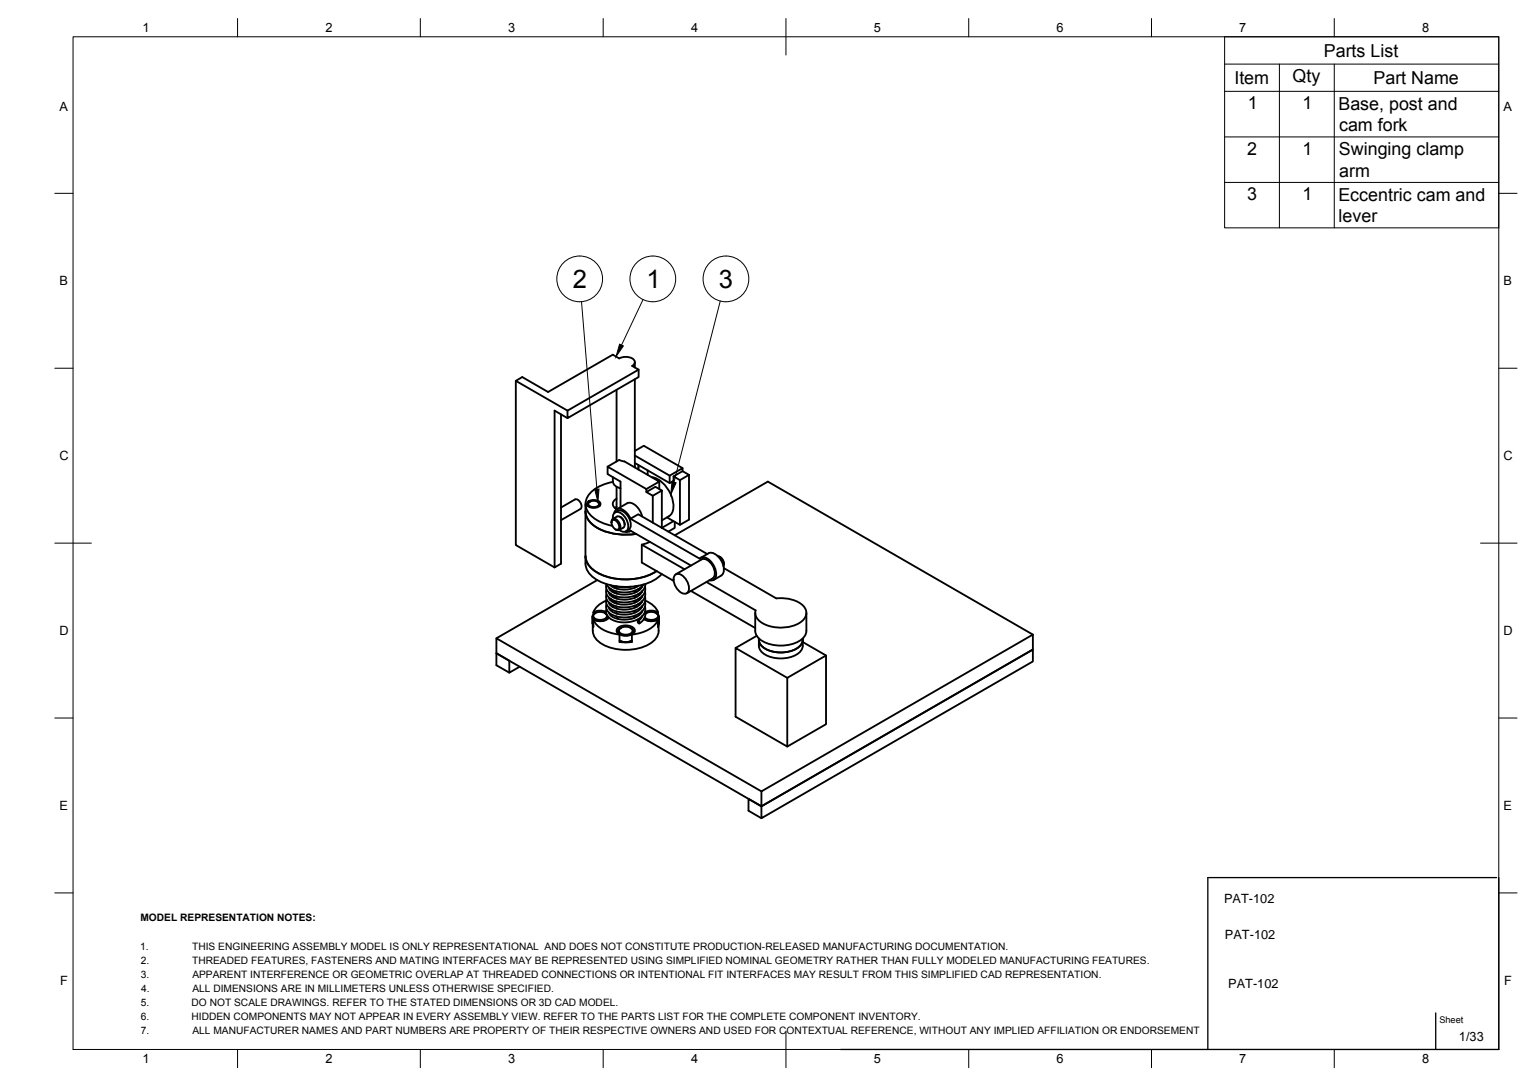
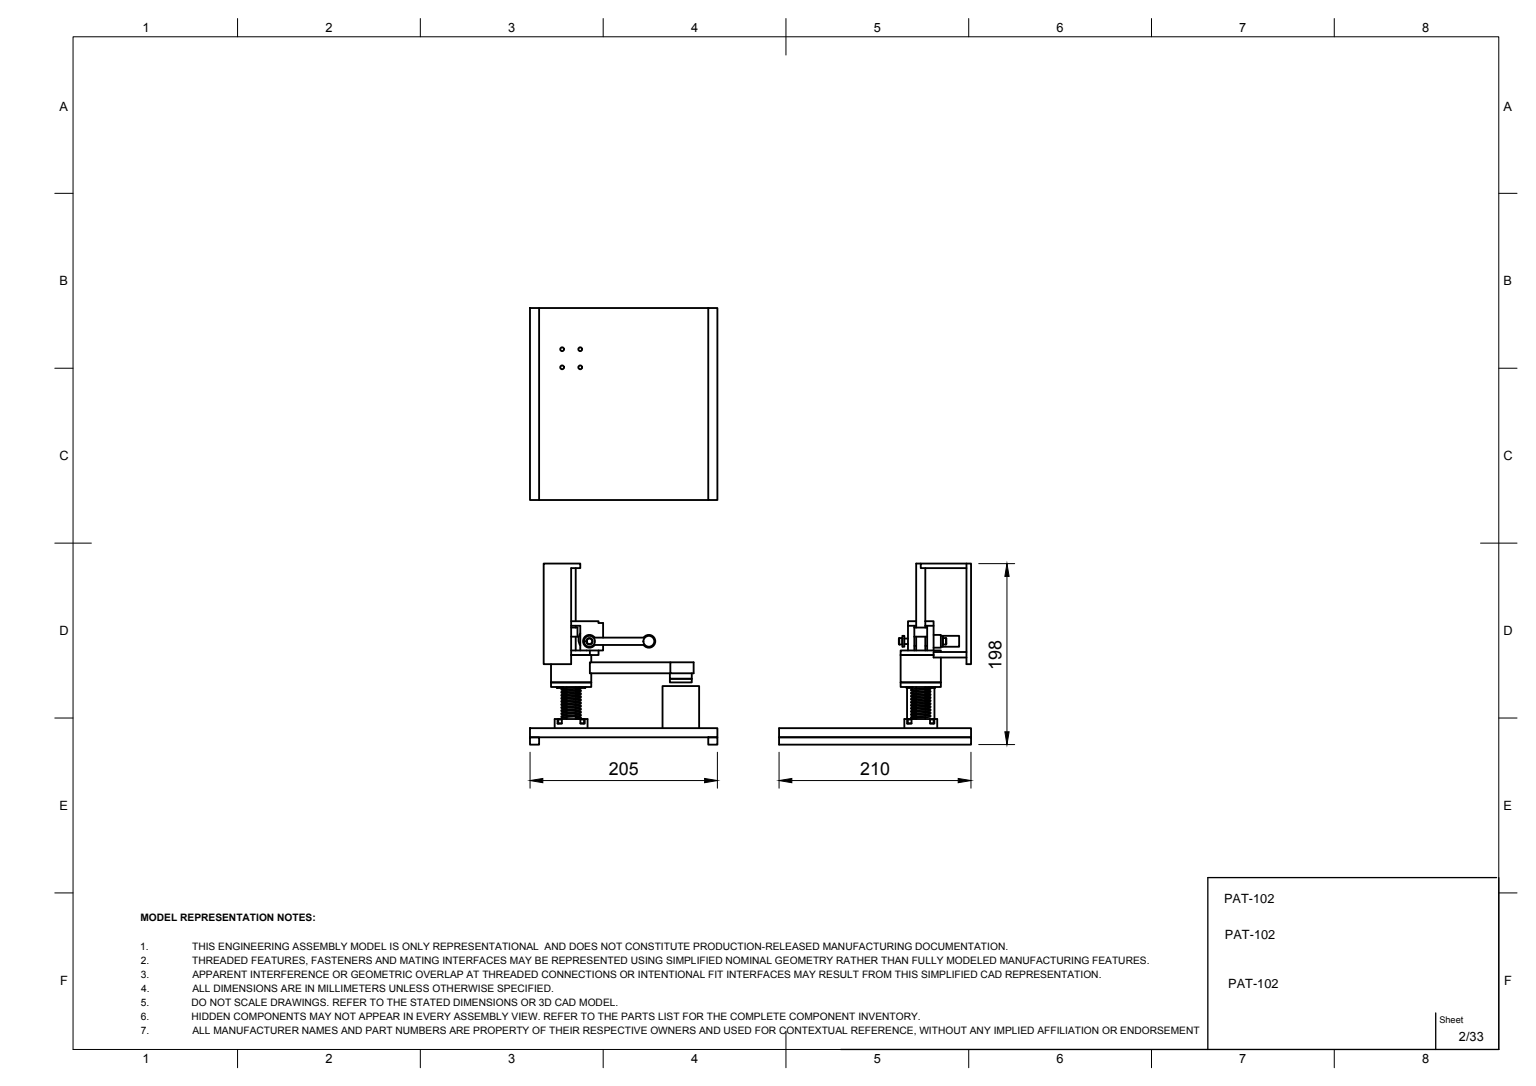
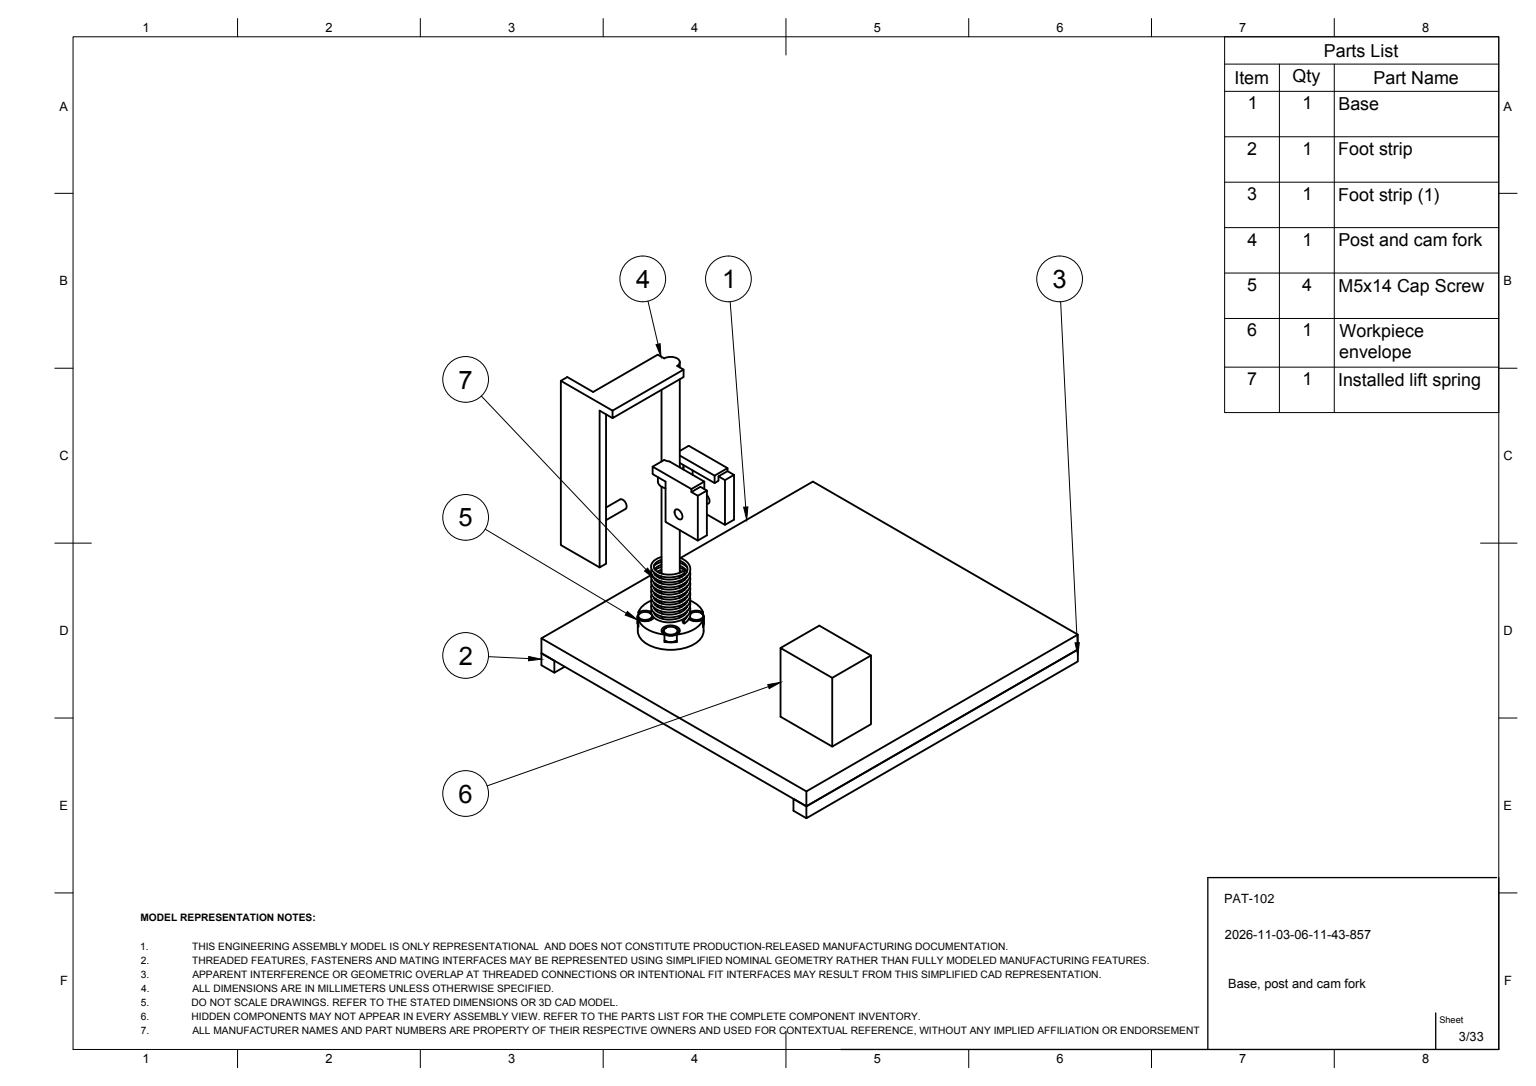
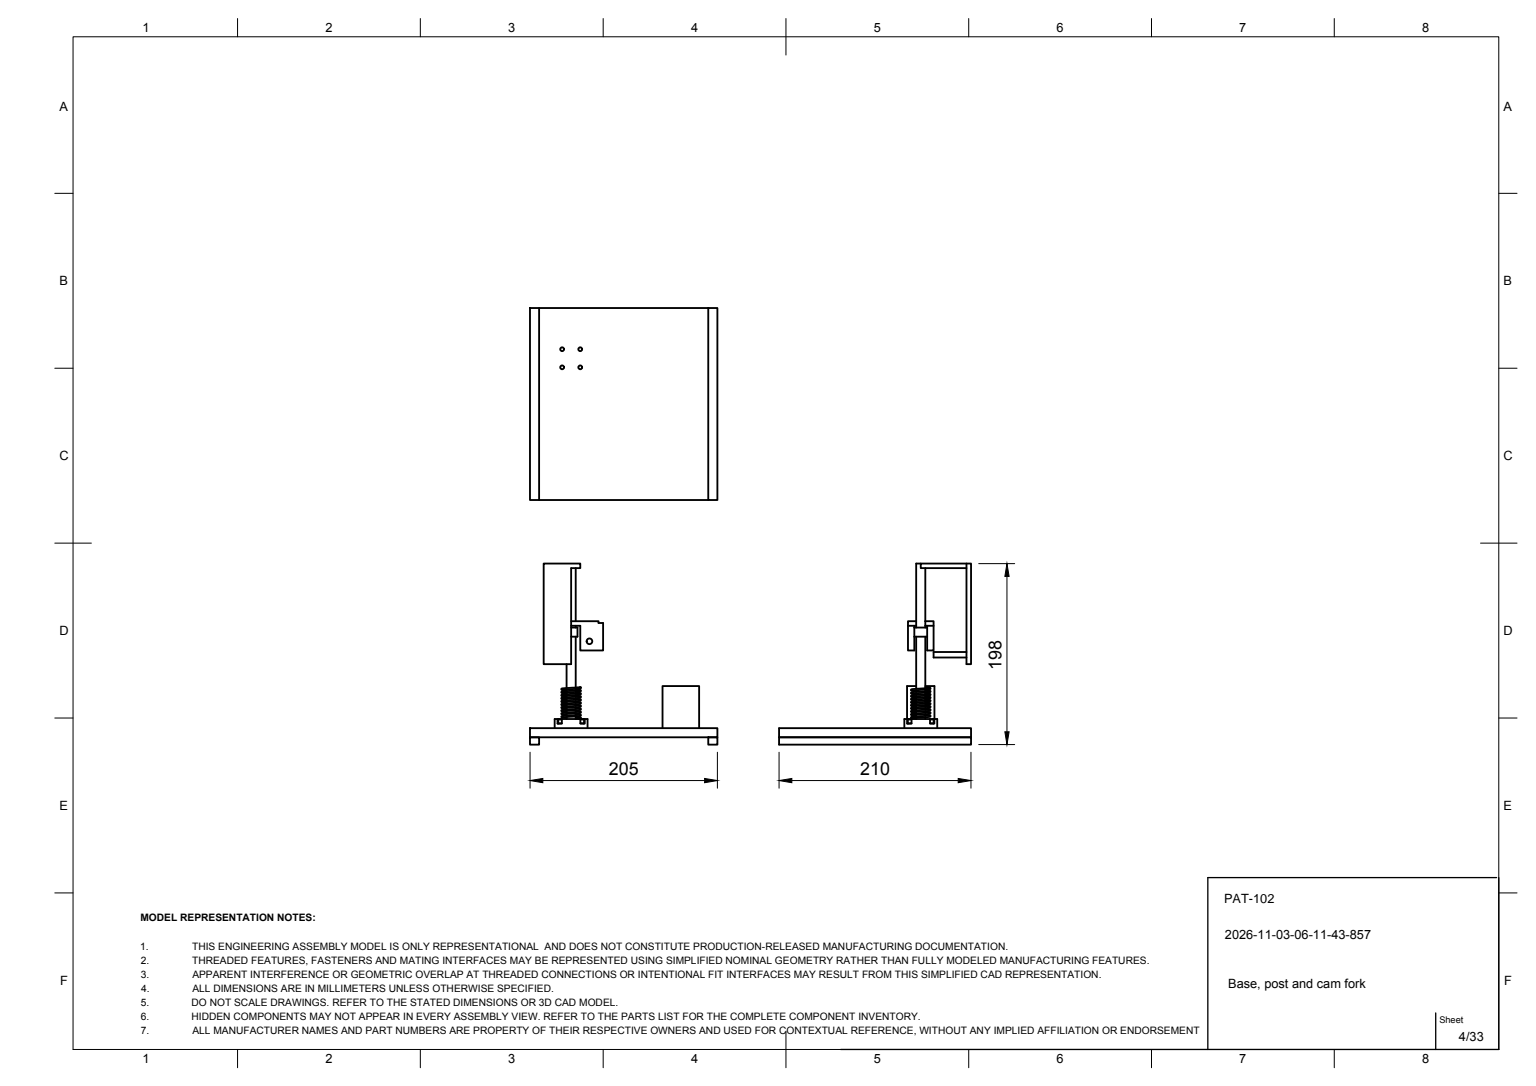
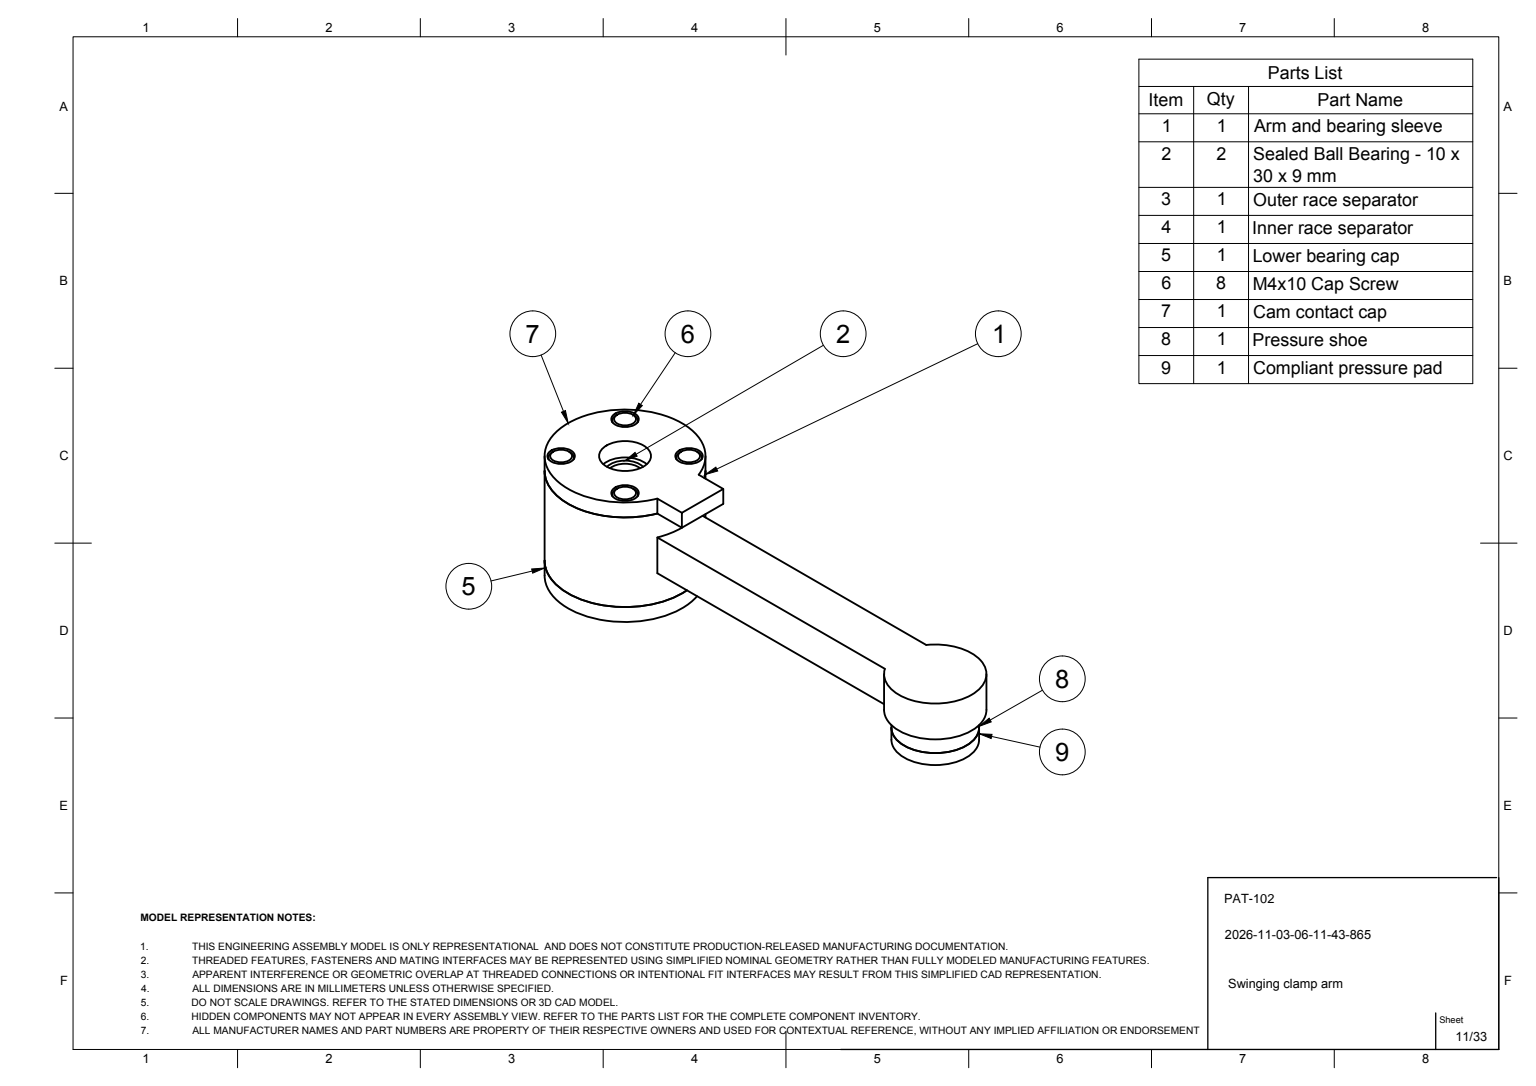
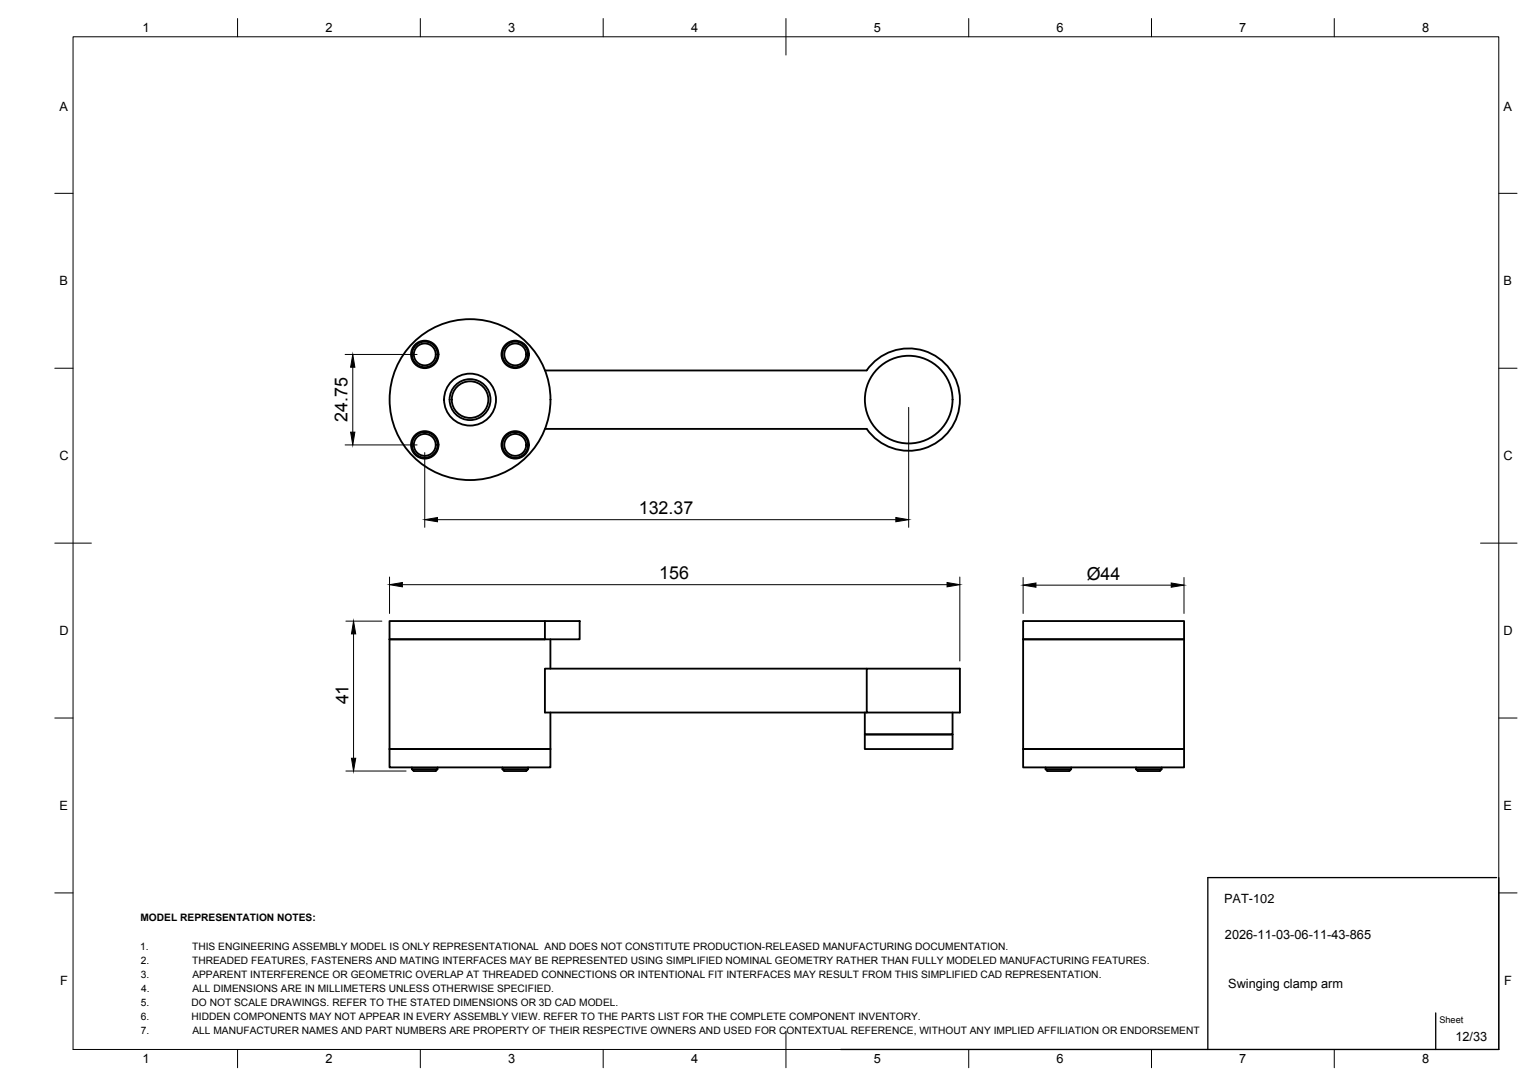
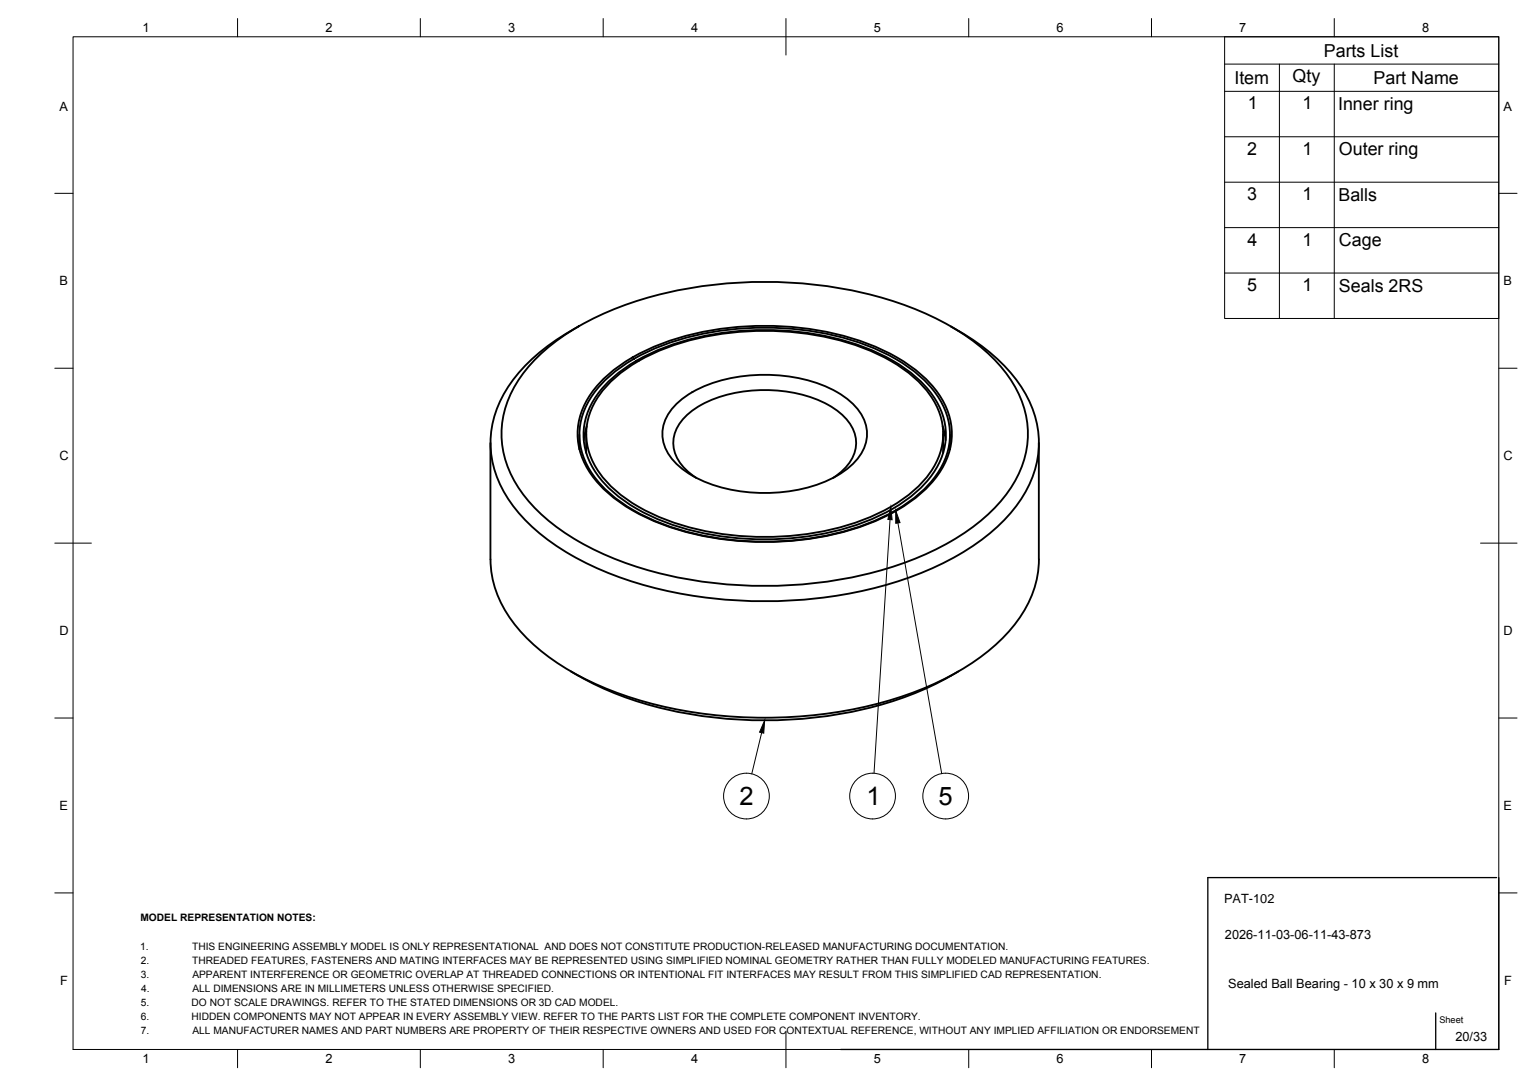
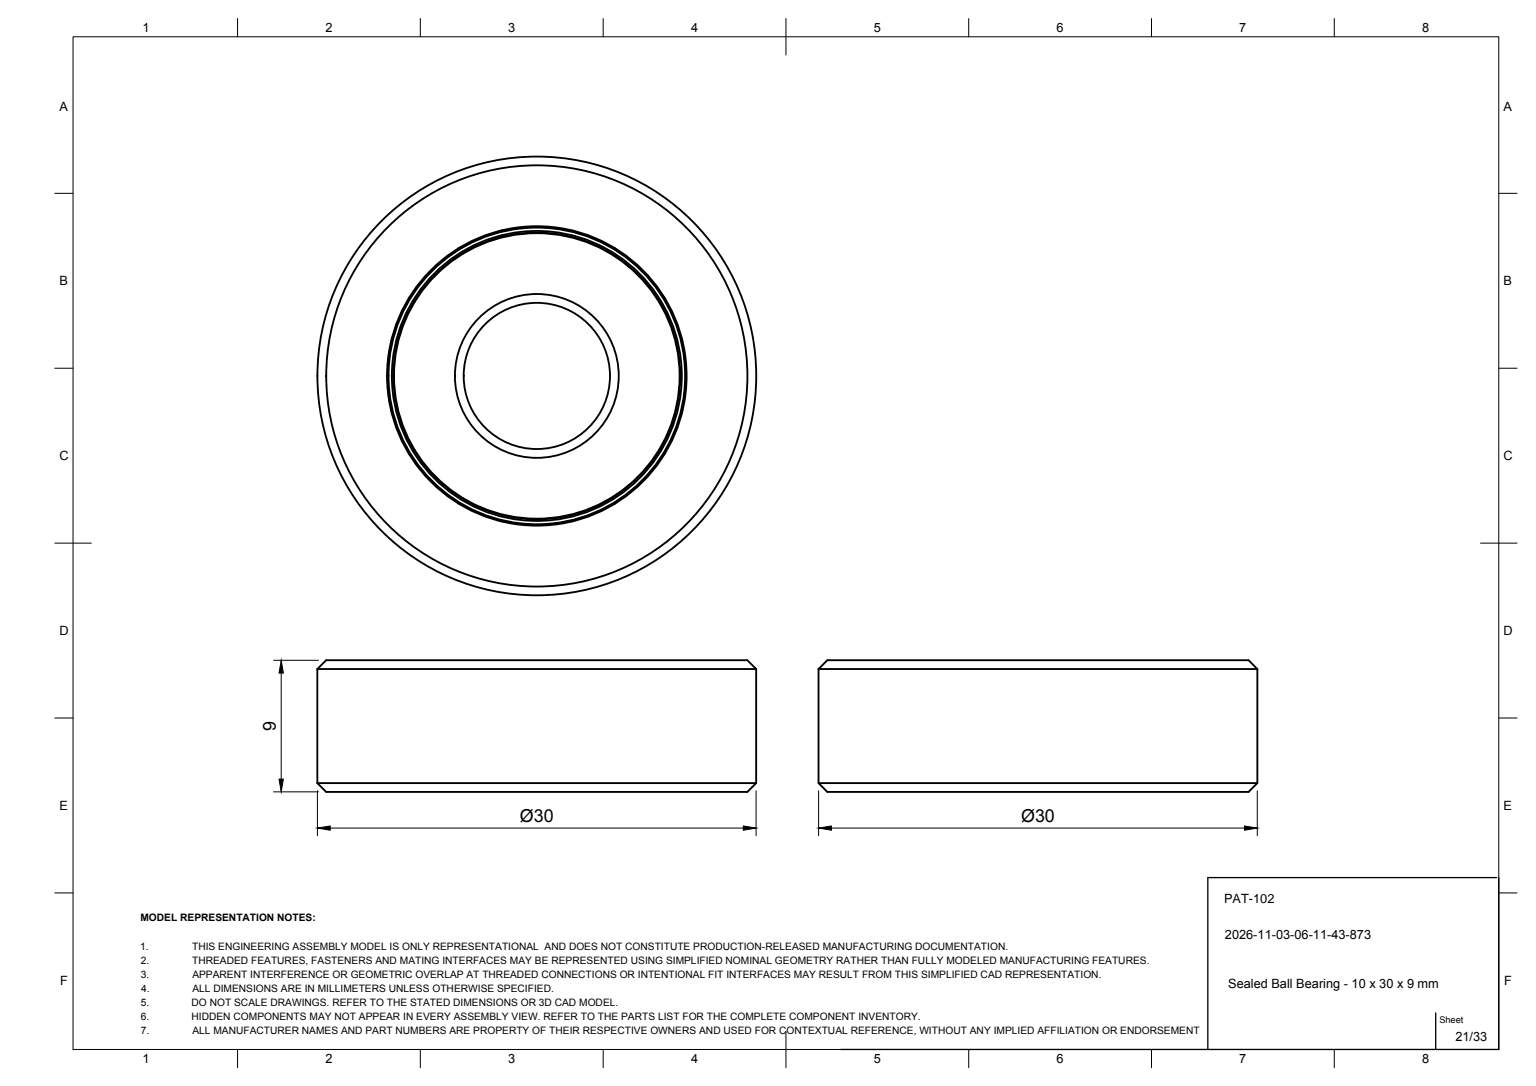
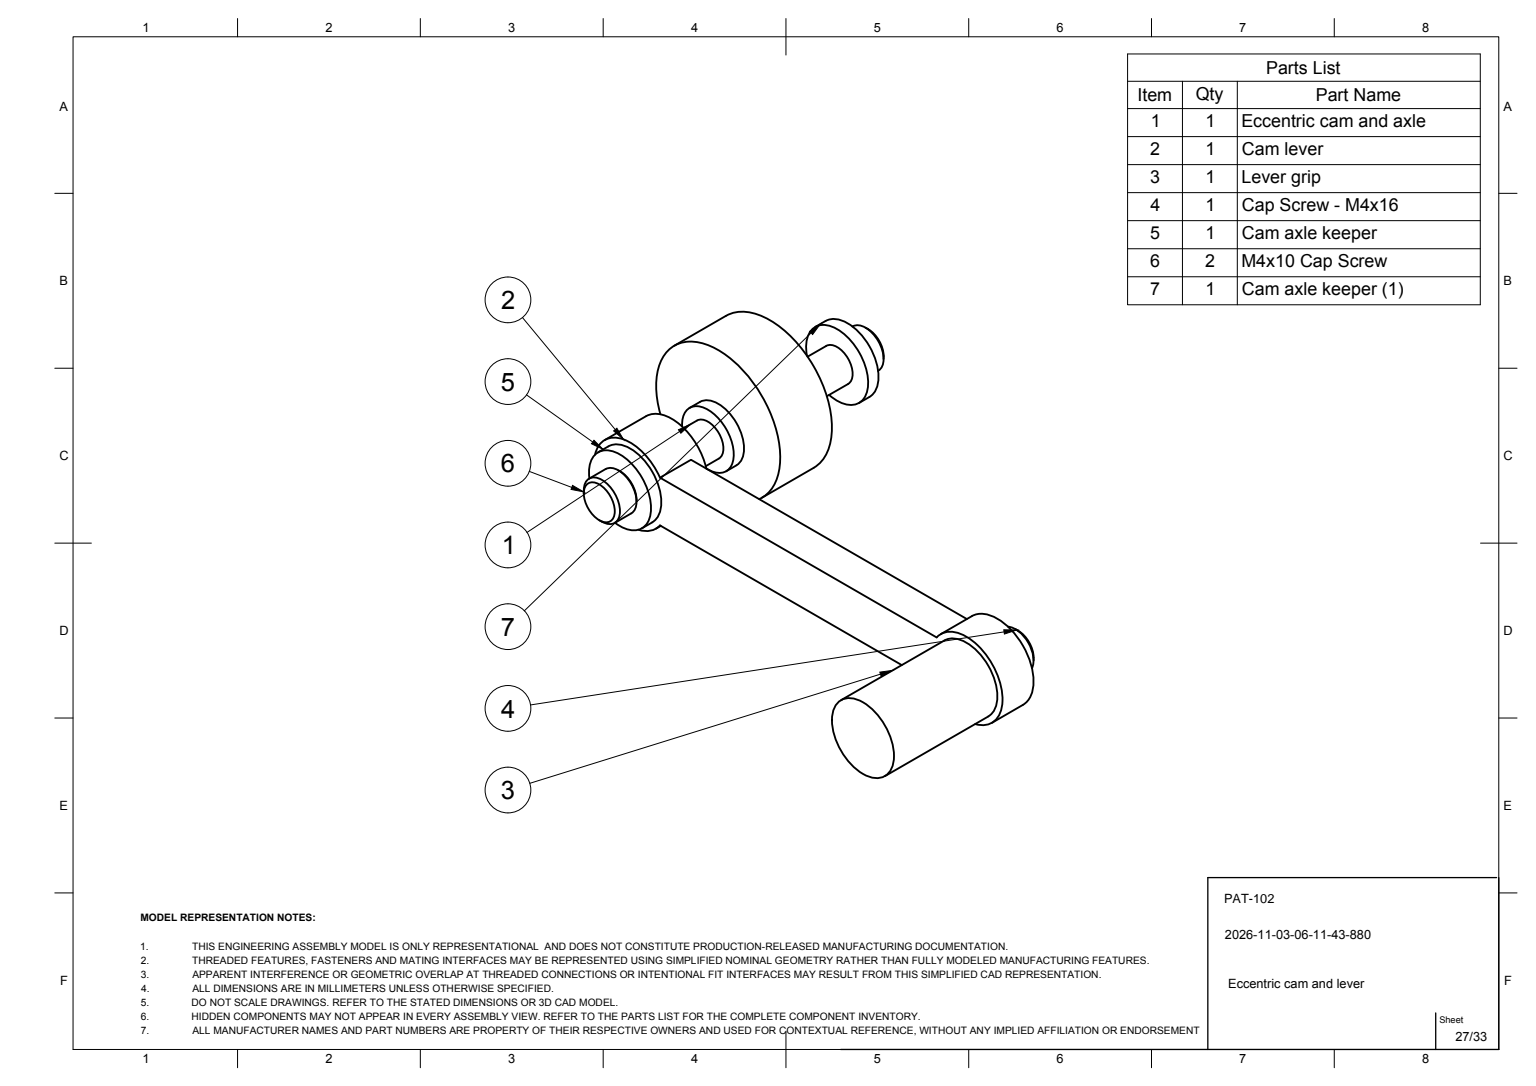
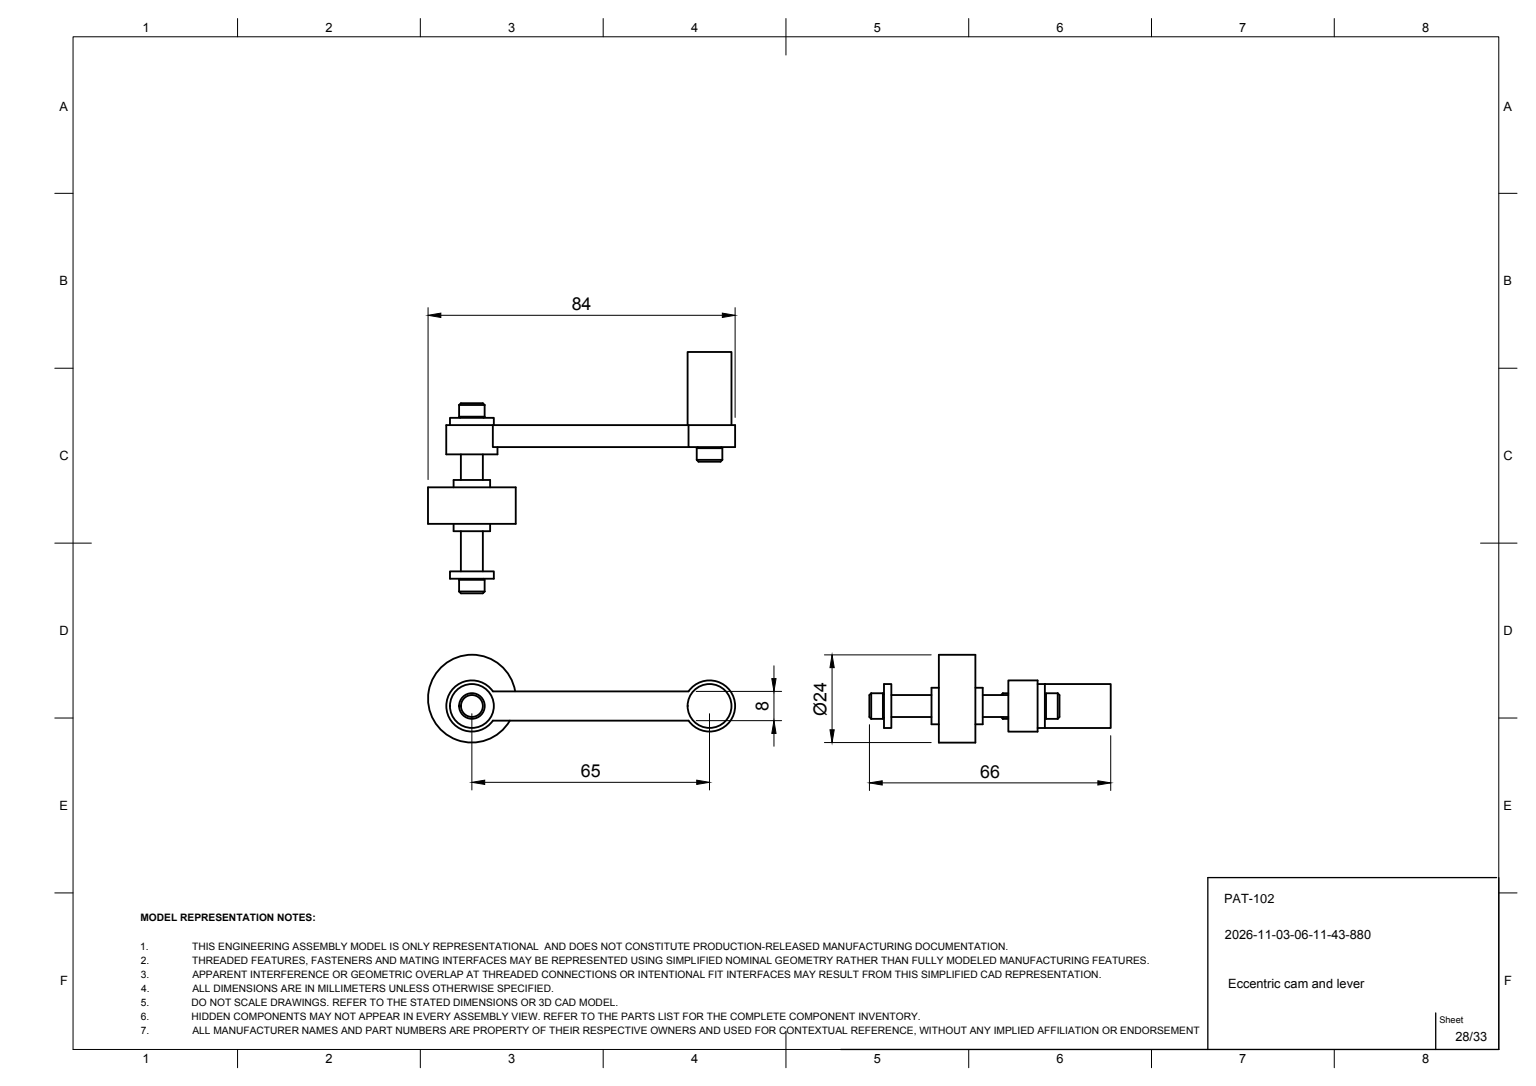
ISO-10303-21;
HEADER;
/* Generated by software containing ST-Developer
 * from STEP Tools, Inc. (www.steptools.com) 
 */

FILE_DESCRIPTION(
/* description */ ('Swing-away clamp arm'),
/* implementation_level */ '2;1');

FILE_NAME(
/* name */ 'PAT-102',
/* time_stamp */ '2026-10-28T03:26:03-07:00',
/* author */ (''),
/* organization */ (''),
/* preprocessor_version */ 'ST-DEVELOPER v20.2',
/* originating_system */ 'Autodesk Translation Framework v15.17.0.0',
/* authorisation */ '');

FILE_SCHEMA (('AUTOMOTIVE_DESIGN { 1 0 10303 214 3 1 1 }'));
ENDSEC;

DATA;
#10=MECHANICAL_DESIGN_GEOMETRIC_PRESENTATION_REPRESENTATION('',(#293,#294,
#295,#296,#297,#298,#299,#300,#301,#302,#303,#304,#305,#306,#307,#308,#309,
#310,#311,#312,#313,#314,#315,#316,#317,#318,#319,#320,#321,#322,#323,#324,
#325,#326),#10627);
#11=SPHERICAL_SURFACE('',#5621,0.23815);
#12=SPHERICAL_SURFACE('',#5623,0.23815);
#13=SPHERICAL_SURFACE('',#5625,0.23815);
#14=SPHERICAL_SURFACE('',#5627,0.23815);
#15=SPHERICAL_SURFACE('',#5629,0.23815);
#16=SPHERICAL_SURFACE('',#5631,0.23815);
#17=SPHERICAL_SURFACE('',#5633,0.23815);
#18=SPHERICAL_SURFACE('',#5635,0.23815);
#19=SPHERICAL_SURFACE('',#5638,0.247676);
#20=SPHERICAL_SURFACE('',#5654,0.247676);
#21=SPHERICAL_SURFACE('',#5659,0.247676);
#22=SPHERICAL_SURFACE('',#5664,0.247676);
#23=SPHERICAL_SURFACE('',#5669,0.247676);
#24=SPHERICAL_SURFACE('',#5674,0.247676);
#25=SPHERICAL_SURFACE('',#5679,0.247676);
#26=SPHERICAL_SURFACE('',#5687,0.247676);
#27=TOROIDAL_SURFACE('',#5581,1.,0.247676);
#28=TOROIDAL_SURFACE('',#5601,1.,0.247676);
#29=ITEM_DEFINED_TRANSFORMATION($,$,#5225,#5395);
#30=ITEM_DEFINED_TRANSFORMATION($,$,#5244,#5396);
#31=ITEM_DEFINED_TRANSFORMATION($,$,#5251,#5397);
#32=ITEM_DEFINED_TRANSFORMATION($,$,#5258,#5398);
#33=ITEM_DEFINED_TRANSFORMATION($,$,#5359,#5399);
#34=ITEM_DEFINED_TRANSFORMATION($,$,#5366,#5400);
#35=ITEM_DEFINED_TRANSFORMATION($,$,#5371,#5401);
#36=ITEM_DEFINED_TRANSFORMATION($,$,#5371,#5402);
#37=ITEM_DEFINED_TRANSFORMATION($,$,#5371,#5403);
#38=ITEM_DEFINED_TRANSFORMATION($,$,#5371,#5404);
#39=ITEM_DEFINED_TRANSFORMATION($,$,#5580,#5708);
#40=ITEM_DEFINED_TRANSFORMATION($,$,#5600,#5709);
#41=ITEM_DEFINED_TRANSFORMATION($,$,#5620,#5710);
#42=ITEM_DEFINED_TRANSFORMATION($,$,#5637,#5711);
#43=ITEM_DEFINED_TRANSFORMATION($,$,#5691,#5712);
#44=ITEM_DEFINED_TRANSFORMATION($,$,#5406,#5842);
#45=ITEM_DEFINED_TRANSFORMATION($,$,#5460,#5843);
#46=ITEM_DEFINED_TRANSFORMATION($,$,#5469,#5844);
#47=ITEM_DEFINED_TRANSFORMATION($,$,#5478,#5845);
#48=ITEM_DEFINED_TRANSFORMATION($,$,#5519,#5846);
#49=ITEM_DEFINED_TRANSFORMATION($,$,#5563,#5847);
#50=ITEM_DEFINED_TRANSFORMATION($,$,#5573,#5848);
#51=ITEM_DEFINED_TRANSFORMATION($,$,#5579,#5849);
#52=ITEM_DEFINED_TRANSFORMATION($,$,#5579,#5850);
#53=ITEM_DEFINED_TRANSFORMATION($,$,#5818,#5851);
#54=ITEM_DEFINED_TRANSFORMATION($,$,#5818,#5852);
#55=ITEM_DEFINED_TRANSFORMATION($,$,#5818,#5853);
#56=ITEM_DEFINED_TRANSFORMATION($,$,#5818,#5854);
#57=ITEM_DEFINED_TRANSFORMATION($,$,#5818,#5855);
#58=ITEM_DEFINED_TRANSFORMATION($,$,#5818,#5856);
#59=ITEM_DEFINED_TRANSFORMATION($,$,#5818,#5857);
#60=ITEM_DEFINED_TRANSFORMATION($,$,#5818,#5858);
#61=ITEM_DEFINED_TRANSFORMATION($,$,#5714,#5859);
#62=ITEM_DEFINED_TRANSFORMATION($,$,#5744,#5860);
#63=ITEM_DEFINED_TRANSFORMATION($,$,#5764,#5861);
#64=ITEM_DEFINED_TRANSFORMATION($,$,#5774,#5862);
#65=ITEM_DEFINED_TRANSFORMATION($,$,#5783,#5863);
#66=ITEM_DEFINED_TRANSFORMATION($,$,#5792,#5864);
#67=ITEM_DEFINED_TRANSFORMATION($,$,#5818,#5865);
#68=ITEM_DEFINED_TRANSFORMATION($,$,#5818,#5866);
#69=ITEM_DEFINED_TRANSFORMATION($,$,#5224,#5867);
#70=ITEM_DEFINED_TRANSFORMATION($,$,#5405,#5868);
#71=ITEM_DEFINED_TRANSFORMATION($,$,#5713,#5869);
#72=(
REPRESENTATION_RELATIONSHIP($,$,#10739,#10738)
REPRESENTATION_RELATIONSHIP_WITH_TRANSFORMATION(#29)
SHAPE_REPRESENTATION_RELATIONSHIP()
);
#73=(
REPRESENTATION_RELATIONSHIP($,$,#10740,#10738)
REPRESENTATION_RELATIONSHIP_WITH_TRANSFORMATION(#30)
SHAPE_REPRESENTATION_RELATIONSHIP()
);
#74=(
REPRESENTATION_RELATIONSHIP($,$,#10741,#10738)
REPRESENTATION_RELATIONSHIP_WITH_TRANSFORMATION(#31)
SHAPE_REPRESENTATION_RELATIONSHIP()
);
#75=(
REPRESENTATION_RELATIONSHIP($,$,#10742,#10738)
REPRESENTATION_RELATIONSHIP_WITH_TRANSFORMATION(#32)
SHAPE_REPRESENTATION_RELATIONSHIP()
);
#76=(
REPRESENTATION_RELATIONSHIP($,$,#10743,#10738)
REPRESENTATION_RELATIONSHIP_WITH_TRANSFORMATION(#33)
SHAPE_REPRESENTATION_RELATIONSHIP()
);
#77=(
REPRESENTATION_RELATIONSHIP($,$,#10744,#10738)
REPRESENTATION_RELATIONSHIP_WITH_TRANSFORMATION(#34)
SHAPE_REPRESENTATION_RELATIONSHIP()
);
#78=(
REPRESENTATION_RELATIONSHIP($,$,#10745,#10738)
REPRESENTATION_RELATIONSHIP_WITH_TRANSFORMATION(#35)
SHAPE_REPRESENTATION_RELATIONSHIP()
);
#79=(
REPRESENTATION_RELATIONSHIP($,$,#10745,#10738)
REPRESENTATION_RELATIONSHIP_WITH_TRANSFORMATION(#36)
SHAPE_REPRESENTATION_RELATIONSHIP()
);
#80=(
REPRESENTATION_RELATIONSHIP($,$,#10745,#10738)
REPRESENTATION_RELATIONSHIP_WITH_TRANSFORMATION(#37)
SHAPE_REPRESENTATION_RELATIONSHIP()
);
#81=(
REPRESENTATION_RELATIONSHIP($,$,#10745,#10738)
REPRESENTATION_RELATIONSHIP_WITH_TRANSFORMATION(#38)
SHAPE_REPRESENTATION_RELATIONSHIP()
);
#82=(
REPRESENTATION_RELATIONSHIP($,$,#10755,#10754)
REPRESENTATION_RELATIONSHIP_WITH_TRANSFORMATION(#39)
SHAPE_REPRESENTATION_RELATIONSHIP()
);
#83=(
REPRESENTATION_RELATIONSHIP($,$,#10756,#10754)
REPRESENTATION_RELATIONSHIP_WITH_TRANSFORMATION(#40)
SHAPE_REPRESENTATION_RELATIONSHIP()
);
#84=(
REPRESENTATION_RELATIONSHIP($,$,#10757,#10754)
REPRESENTATION_RELATIONSHIP_WITH_TRANSFORMATION(#41)
SHAPE_REPRESENTATION_RELATIONSHIP()
);
#85=(
REPRESENTATION_RELATIONSHIP($,$,#10758,#10754)
REPRESENTATION_RELATIONSHIP_WITH_TRANSFORMATION(#42)
SHAPE_REPRESENTATION_RELATIONSHIP()
);
#86=(
REPRESENTATION_RELATIONSHIP($,$,#10759,#10754)
REPRESENTATION_RELATIONSHIP_WITH_TRANSFORMATION(#43)
SHAPE_REPRESENTATION_RELATIONSHIP()
);
#87=(
REPRESENTATION_RELATIONSHIP($,$,#10747,#10746)
REPRESENTATION_RELATIONSHIP_WITH_TRANSFORMATION(#44)
SHAPE_REPRESENTATION_RELATIONSHIP()
);
#88=(
REPRESENTATION_RELATIONSHIP($,$,#10748,#10746)
REPRESENTATION_RELATIONSHIP_WITH_TRANSFORMATION(#45)
SHAPE_REPRESENTATION_RELATIONSHIP()
);
#89=(
REPRESENTATION_RELATIONSHIP($,$,#10749,#10746)
REPRESENTATION_RELATIONSHIP_WITH_TRANSFORMATION(#46)
SHAPE_REPRESENTATION_RELATIONSHIP()
);
#90=(
REPRESENTATION_RELATIONSHIP($,$,#10750,#10746)
REPRESENTATION_RELATIONSHIP_WITH_TRANSFORMATION(#47)
SHAPE_REPRESENTATION_RELATIONSHIP()
);
#91=(
REPRESENTATION_RELATIONSHIP($,$,#10751,#10746)
REPRESENTATION_RELATIONSHIP_WITH_TRANSFORMATION(#48)
SHAPE_REPRESENTATION_RELATIONSHIP()
);
#92=(
REPRESENTATION_RELATIONSHIP($,$,#10752,#10746)
REPRESENTATION_RELATIONSHIP_WITH_TRANSFORMATION(#49)
SHAPE_REPRESENTATION_RELATIONSHIP()
);
#93=(
REPRESENTATION_RELATIONSHIP($,$,#10753,#10746)
REPRESENTATION_RELATIONSHIP_WITH_TRANSFORMATION(#50)
SHAPE_REPRESENTATION_RELATIONSHIP()
);
#94=(
REPRESENTATION_RELATIONSHIP($,$,#10754,#10746)
REPRESENTATION_RELATIONSHIP_WITH_TRANSFORMATION(#51)
SHAPE_REPRESENTATION_RELATIONSHIP()
);
#95=(
REPRESENTATION_RELATIONSHIP($,$,#10754,#10746)
REPRESENTATION_RELATIONSHIP_WITH_TRANSFORMATION(#52)
SHAPE_REPRESENTATION_RELATIONSHIP()
);
#96=(
REPRESENTATION_RELATIONSHIP($,$,#10767,#10746)
REPRESENTATION_RELATIONSHIP_WITH_TRANSFORMATION(#53)
SHAPE_REPRESENTATION_RELATIONSHIP()
);
#97=(
REPRESENTATION_RELATIONSHIP($,$,#10767,#10746)
REPRESENTATION_RELATIONSHIP_WITH_TRANSFORMATION(#54)
SHAPE_REPRESENTATION_RELATIONSHIP()
);
#98=(
REPRESENTATION_RELATIONSHIP($,$,#10767,#10746)
REPRESENTATION_RELATIONSHIP_WITH_TRANSFORMATION(#55)
SHAPE_REPRESENTATION_RELATIONSHIP()
);
#99=(
REPRESENTATION_RELATIONSHIP($,$,#10767,#10746)
REPRESENTATION_RELATIONSHIP_WITH_TRANSFORMATION(#56)
SHAPE_REPRESENTATION_RELATIONSHIP()
);
#100=(
REPRESENTATION_RELATIONSHIP($,$,#10767,#10746)
REPRESENTATION_RELATIONSHIP_WITH_TRANSFORMATION(#57)
SHAPE_REPRESENTATION_RELATIONSHIP()
);
#101=(
REPRESENTATION_RELATIONSHIP($,$,#10767,#10746)
REPRESENTATION_RELATIONSHIP_WITH_TRANSFORMATION(#58)
SHAPE_REPRESENTATION_RELATIONSHIP()
);
#102=(
REPRESENTATION_RELATIONSHIP($,$,#10767,#10746)
REPRESENTATION_RELATIONSHIP_WITH_TRANSFORMATION(#59)
SHAPE_REPRESENTATION_RELATIONSHIP()
);
#103=(
REPRESENTATION_RELATIONSHIP($,$,#10767,#10746)
REPRESENTATION_RELATIONSHIP_WITH_TRANSFORMATION(#60)
SHAPE_REPRESENTATION_RELATIONSHIP()
);
#104=(
REPRESENTATION_RELATIONSHIP($,$,#10761,#10760)
REPRESENTATION_RELATIONSHIP_WITH_TRANSFORMATION(#61)
SHAPE_REPRESENTATION_RELATIONSHIP()
);
#105=(
REPRESENTATION_RELATIONSHIP($,$,#10762,#10760)
REPRESENTATION_RELATIONSHIP_WITH_TRANSFORMATION(#62)
SHAPE_REPRESENTATION_RELATIONSHIP()
);
#106=(
REPRESENTATION_RELATIONSHIP($,$,#10763,#10760)
REPRESENTATION_RELATIONSHIP_WITH_TRANSFORMATION(#63)
SHAPE_REPRESENTATION_RELATIONSHIP()
);
#107=(
REPRESENTATION_RELATIONSHIP($,$,#10764,#10760)
REPRESENTATION_RELATIONSHIP_WITH_TRANSFORMATION(#64)
SHAPE_REPRESENTATION_RELATIONSHIP()
);
#108=(
REPRESENTATION_RELATIONSHIP($,$,#10765,#10760)
REPRESENTATION_RELATIONSHIP_WITH_TRANSFORMATION(#65)
SHAPE_REPRESENTATION_RELATIONSHIP()
);
#109=(
REPRESENTATION_RELATIONSHIP($,$,#10766,#10760)
REPRESENTATION_RELATIONSHIP_WITH_TRANSFORMATION(#66)
SHAPE_REPRESENTATION_RELATIONSHIP()
);
#110=(
REPRESENTATION_RELATIONSHIP($,$,#10767,#10760)
REPRESENTATION_RELATIONSHIP_WITH_TRANSFORMATION(#67)
SHAPE_REPRESENTATION_RELATIONSHIP()
);
#111=(
REPRESENTATION_RELATIONSHIP($,$,#10767,#10760)
REPRESENTATION_RELATIONSHIP_WITH_TRANSFORMATION(#68)
SHAPE_REPRESENTATION_RELATIONSHIP()
);
#112=(
REPRESENTATION_RELATIONSHIP($,$,#10738,#10737)
REPRESENTATION_RELATIONSHIP_WITH_TRANSFORMATION(#69)
SHAPE_REPRESENTATION_RELATIONSHIP()
);
#113=(
REPRESENTATION_RELATIONSHIP($,$,#10746,#10737)
REPRESENTATION_RELATIONSHIP_WITH_TRANSFORMATION(#70)
SHAPE_REPRESENTATION_RELATIONSHIP()
);
#114=(
REPRESENTATION_RELATIONSHIP($,$,#10760,#10737)
REPRESENTATION_RELATIONSHIP_WITH_TRANSFORMATION(#71)
SHAPE_REPRESENTATION_RELATIONSHIP()
);
#115=CONTEXT_DEPENDENT_SHAPE_REPRESENTATION(#72,#10672);
#116=CONTEXT_DEPENDENT_SHAPE_REPRESENTATION(#73,#10673);
#117=CONTEXT_DEPENDENT_SHAPE_REPRESENTATION(#74,#10674);
#118=CONTEXT_DEPENDENT_SHAPE_REPRESENTATION(#75,#10675);
#119=CONTEXT_DEPENDENT_SHAPE_REPRESENTATION(#76,#10676);
#120=CONTEXT_DEPENDENT_SHAPE_REPRESENTATION(#77,#10677);
#121=CONTEXT_DEPENDENT_SHAPE_REPRESENTATION(#78,#10678);
#122=CONTEXT_DEPENDENT_SHAPE_REPRESENTATION(#79,#10679);
#123=CONTEXT_DEPENDENT_SHAPE_REPRESENTATION(#80,#10680);
#124=CONTEXT_DEPENDENT_SHAPE_REPRESENTATION(#81,#10681);
#125=CONTEXT_DEPENDENT_SHAPE_REPRESENTATION(#82,#10696);
#126=CONTEXT_DEPENDENT_SHAPE_REPRESENTATION(#83,#10697);
#127=CONTEXT_DEPENDENT_SHAPE_REPRESENTATION(#84,#10698);
#128=CONTEXT_DEPENDENT_SHAPE_REPRESENTATION(#85,#10699);
#129=CONTEXT_DEPENDENT_SHAPE_REPRESENTATION(#86,#10700);
#130=CONTEXT_DEPENDENT_SHAPE_REPRESENTATION(#87,#10709);
#131=CONTEXT_DEPENDENT_SHAPE_REPRESENTATION(#88,#10710);
#132=CONTEXT_DEPENDENT_SHAPE_REPRESENTATION(#89,#10711);
#133=CONTEXT_DEPENDENT_SHAPE_REPRESENTATION(#90,#10712);
#134=CONTEXT_DEPENDENT_SHAPE_REPRESENTATION(#91,#10713);
#135=CONTEXT_DEPENDENT_SHAPE_REPRESENTATION(#92,#10714);
#136=CONTEXT_DEPENDENT_SHAPE_REPRESENTATION(#93,#10715);
#137=CONTEXT_DEPENDENT_SHAPE_REPRESENTATION(#94,#10716);
#138=CONTEXT_DEPENDENT_SHAPE_REPRESENTATION(#95,#10717);
#139=CONTEXT_DEPENDENT_SHAPE_REPRESENTATION(#96,#10718);
#140=CONTEXT_DEPENDENT_SHAPE_REPRESENTATION(#97,#10719);
#141=CONTEXT_DEPENDENT_SHAPE_REPRESENTATION(#98,#10720);
#142=CONTEXT_DEPENDENT_SHAPE_REPRESENTATION(#99,#10721);
#143=CONTEXT_DEPENDENT_SHAPE_REPRESENTATION(#100,#10722);
#144=CONTEXT_DEPENDENT_SHAPE_REPRESENTATION(#101,#10723);
#145=CONTEXT_DEPENDENT_SHAPE_REPRESENTATION(#102,#10724);
#146=CONTEXT_DEPENDENT_SHAPE_REPRESENTATION(#103,#10725);
#147=CONTEXT_DEPENDENT_SHAPE_REPRESENTATION(#104,#10726);
#148=CONTEXT_DEPENDENT_SHAPE_REPRESENTATION(#105,#10727);
#149=CONTEXT_DEPENDENT_SHAPE_REPRESENTATION(#106,#10728);
#150=CONTEXT_DEPENDENT_SHAPE_REPRESENTATION(#107,#10729);
#151=CONTEXT_DEPENDENT_SHAPE_REPRESENTATION(#108,#10730);
#152=CONTEXT_DEPENDENT_SHAPE_REPRESENTATION(#109,#10731);
#153=CONTEXT_DEPENDENT_SHAPE_REPRESENTATION(#110,#10732);
#154=CONTEXT_DEPENDENT_SHAPE_REPRESENTATION(#111,#10733);
#155=CONTEXT_DEPENDENT_SHAPE_REPRESENTATION(#112,#10734);
#156=CONTEXT_DEPENDENT_SHAPE_REPRESENTATION(#113,#10735);
#157=CONTEXT_DEPENDENT_SHAPE_REPRESENTATION(#114,#10736);
#158=NEXT_ASSEMBLY_USAGE_OCCURRENCE('Base:1','Base:1','Base:1',#10770,#10771,
'Base:1');
#159=NEXT_ASSEMBLY_USAGE_OCCURRENCE('Foot strip:1','Foot strip:1',
'Foot strip:1',#10770,#10772,'Foot strip:1');
#160=NEXT_ASSEMBLY_USAGE_OCCURRENCE('Foot strip (1):1',
'Foot strip (1):1','Foot strip (1):1',#10770,#10773,'Foot strip (1):1');
#161=NEXT_ASSEMBLY_USAGE_OCCURRENCE('Post and cam fork:1',
'Post and cam fork:1','Post and cam fork:1',#10770,#10774,
'Post and cam fork:1');
#162=NEXT_ASSEMBLY_USAGE_OCCURRENCE('Workpiece envelope:1',
'Workpiece envelope:1','Workpiece envelope:1',#10770,#10775,
'Workpiece envelope:1');
#163=NEXT_ASSEMBLY_USAGE_OCCURRENCE('Installed lift spring:1',
'Installed lift spring:1','Installed lift spring:1',#10770,#10776,
'Installed lift spring:1');
#164=NEXT_ASSEMBLY_USAGE_OCCURRENCE('M5x14 Cap Screw:2',
'M5x14 Cap Screw:2','M5x14 Cap Screw:2',#10770,#10777,
'M5x14 Cap Screw:2');
#165=NEXT_ASSEMBLY_USAGE_OCCURRENCE('M5x14 Cap Screw:3',
'M5x14 Cap Screw:3','M5x14 Cap Screw:3',#10770,#10777,
'M5x14 Cap Screw:3');
#166=NEXT_ASSEMBLY_USAGE_OCCURRENCE('M5x14 Cap Screw:4',
'M5x14 Cap Screw:4','M5x14 Cap Screw:4',#10770,#10777,
'M5x14 Cap Screw:4');
#167=NEXT_ASSEMBLY_USAGE_OCCURRENCE('M5x14 Cap Screw:5',
'M5x14 Cap Screw:5','M5x14 Cap Screw:5',#10770,#10777,
'M5x14 Cap Screw:5');
#168=NEXT_ASSEMBLY_USAGE_OCCURRENCE('Inner ring:1','Inner ring:1',
'Inner ring:1',#10786,#10787,'Inner ring:1');
#169=NEXT_ASSEMBLY_USAGE_OCCURRENCE('Outer ring:1','Outer ring:1',
'Outer ring:1',#10786,#10788,'Outer ring:1');
#170=NEXT_ASSEMBLY_USAGE_OCCURRENCE('Balls:1','Balls:1','Balls:1',#10786,
#10789,'Balls:1');
#171=NEXT_ASSEMBLY_USAGE_OCCURRENCE('Cage:1','Cage:1','Cage:1',#10786,#10790,
'Cage:1');
#172=NEXT_ASSEMBLY_USAGE_OCCURRENCE('Seals 2RS:1','Seals 2RS:1',
'Seals 2RS:1',#10786,#10791,'Seals 2RS:1');
#173=NEXT_ASSEMBLY_USAGE_OCCURRENCE('Arm and bearing sleeve:1',
'Arm and bearing sleeve:1','Arm and bearing sleeve:1',#10778,#10779,
'Arm and bearing sleeve:1');
#174=NEXT_ASSEMBLY_USAGE_OCCURRENCE('Outer race separator:1',
'Outer race separator:1','Outer race separator:1',#10778,#10780,
'Outer race separator:1');
#175=NEXT_ASSEMBLY_USAGE_OCCURRENCE('Inner race separator:1',
'Inner race separator:1','Inner race separator:1',#10778,#10781,
'Inner race separator:1');
#176=NEXT_ASSEMBLY_USAGE_OCCURRENCE('Lower bearing cap:1',
'Lower bearing cap:1','Lower bearing cap:1',#10778,#10782,
'Lower bearing cap:1');
#177=NEXT_ASSEMBLY_USAGE_OCCURRENCE('Cam contact cap:1',
'Cam contact cap:1','Cam contact cap:1',#10778,#10783,
'Cam contact cap:1');
#178=NEXT_ASSEMBLY_USAGE_OCCURRENCE('Pressure shoe:1','Pressure shoe:1',
'Pressure shoe:1',#10778,#10784,'Pressure shoe:1');
#179=NEXT_ASSEMBLY_USAGE_OCCURRENCE('Compliant pressure pad:1',
'Compliant pressure pad:1','Compliant pressure pad:1',#10778,#10785,
'Compliant pressure pad:1');
#180=NEXT_ASSEMBLY_USAGE_OCCURRENCE(
'Sealed Ball Bearing - 10 x 30 x 9 mm:2',
'Sealed Ball Bearing - 10 x 30 x 9 mm:2',
'Sealed Ball Bearing - 10 x 30 x 9 mm:2',#10778,#10786,
'Sealed Ball Bearing - 10 x 30 x 9 mm:2');
#181=NEXT_ASSEMBLY_USAGE_OCCURRENCE(
'Sealed Ball Bearing - 10 x 30 x 9 mm:3',
'Sealed Ball Bearing - 10 x 30 x 9 mm:3',
'Sealed Ball Bearing - 10 x 30 x 9 mm:3',#10778,#10786,
'Sealed Ball Bearing - 10 x 30 x 9 mm:3');
#182=NEXT_ASSEMBLY_USAGE_OCCURRENCE('M4x10 Cap Screw:2',
'M4x10 Cap Screw:2','M4x10 Cap Screw:2',#10778,#10799,
'M4x10 Cap Screw:2');
#183=NEXT_ASSEMBLY_USAGE_OCCURRENCE('M4x10 Cap Screw:3',
'M4x10 Cap Screw:3','M4x10 Cap Screw:3',#10778,#10799,
'M4x10 Cap Screw:3');
#184=NEXT_ASSEMBLY_USAGE_OCCURRENCE('M4x10 Cap Screw:4',
'M4x10 Cap Screw:4','M4x10 Cap Screw:4',#10778,#10799,
'M4x10 Cap Screw:4');
#185=NEXT_ASSEMBLY_USAGE_OCCURRENCE('M4x10 Cap Screw:5',
'M4x10 Cap Screw:5','M4x10 Cap Screw:5',#10778,#10799,
'M4x10 Cap Screw:5');
#186=NEXT_ASSEMBLY_USAGE_OCCURRENCE('M4x10 Cap Screw:6',
'M4x10 Cap Screw:6','M4x10 Cap Screw:6',#10778,#10799,
'M4x10 Cap Screw:6');
#187=NEXT_ASSEMBLY_USAGE_OCCURRENCE('M4x10 Cap Screw:7',
'M4x10 Cap Screw:7','M4x10 Cap Screw:7',#10778,#10799,
'M4x10 Cap Screw:7');
#188=NEXT_ASSEMBLY_USAGE_OCCURRENCE('M4x10 Cap Screw:8',
'M4x10 Cap Screw:8','M4x10 Cap Screw:8',#10778,#10799,
'M4x10 Cap Screw:8');
#189=NEXT_ASSEMBLY_USAGE_OCCURRENCE('M4x10 Cap Screw:9',
'M4x10 Cap Screw:9','M4x10 Cap Screw:9',#10778,#10799,
'M4x10 Cap Screw:9');
#190=NEXT_ASSEMBLY_USAGE_OCCURRENCE('Eccentric cam and axle:1',
'Eccentric cam and axle:1','Eccentric cam and axle:1',#10792,#10793,
'Eccentric cam and axle:1');
#191=NEXT_ASSEMBLY_USAGE_OCCURRENCE('Cam lever:1','Cam lever:1',
'Cam lever:1',#10792,#10794,'Cam lever:1');
#192=NEXT_ASSEMBLY_USAGE_OCCURRENCE('Lever grip:1','Lever grip:1',
'Lever grip:1',#10792,#10795,'Lever grip:1');
#193=NEXT_ASSEMBLY_USAGE_OCCURRENCE('Cam axle keeper:1',
'Cam axle keeper:1','Cam axle keeper:1',#10792,#10796,
'Cam axle keeper:1');
#194=NEXT_ASSEMBLY_USAGE_OCCURRENCE('Cam axle keeper (1):1',
'Cam axle keeper (1):1','Cam axle keeper (1):1',#10792,#10797,
'Cam axle keeper (1):1');
#195=NEXT_ASSEMBLY_USAGE_OCCURRENCE('Cap Screw - M4x16:2',
'Cap Screw - M4x16:2','Cap Screw - M4x16:2',#10792,#10798,
'Cap Screw - M4x16:2');
#196=NEXT_ASSEMBLY_USAGE_OCCURRENCE('M4x10 Cap Screw:10',
'M4x10 Cap Screw:10','M4x10 Cap Screw:10',#10792,#10799,
'M4x10 Cap Screw:10');
#197=NEXT_ASSEMBLY_USAGE_OCCURRENCE('M4x10 Cap Screw:11',
'M4x10 Cap Screw:11','M4x10 Cap Screw:11',#10792,#10799,
'M4x10 Cap Screw:11');
#198=NEXT_ASSEMBLY_USAGE_OCCURRENCE('Base, post and cam fork:1',
'Base, post and cam fork:1','Base, post and cam fork:1',#10769,#10770,
'Base, post and cam fork:1');
#199=NEXT_ASSEMBLY_USAGE_OCCURRENCE('Swinging clamp arm:1',
'Swinging clamp arm:1','Swinging clamp arm:1',#10769,#10778,
'Swinging clamp arm:1');
#200=NEXT_ASSEMBLY_USAGE_OCCURRENCE('Eccentric cam and lever:1',
'Eccentric cam and lever:1','Eccentric cam and lever:1',#10769,#10792,
'Eccentric cam and lever:1');
#201=CONICAL_SURFACE('',#5384,0.4,0.785398163397448);
#202=CONICAL_SURFACE('',#5388,0.41,0.785398163397448);
#203=CONICAL_SURFACE('',#5392,0.26,0.463647609000806);
#204=CONICAL_SURFACE('',#5592,0.53,0.785398163397448);
#205=CONICAL_SURFACE('',#5599,0.53,0.785398163397448);
#206=CONICAL_SURFACE('',#5612,1.47,0.785398163397449);
#207=CONICAL_SURFACE('',#5616,1.47,0.785398163397449);
#208=CONICAL_SURFACE('',#5795,0.325,0.785398163397448);
#209=CONICAL_SURFACE('',#5799,0.335,0.785398163397448);
#210=CONICAL_SURFACE('',#5803,0.21,0.463647609000806);
#211=CONICAL_SURFACE('',#5807,0.18,0.785398163397448);
#212=CONICAL_SURFACE('',#5831,0.325,0.785398163397448);
#213=CONICAL_SURFACE('',#5835,0.335,0.785398163397448);
#214=CONICAL_SURFACE('',#5839,0.21,0.463647609000806);
#215=ORIENTED_CLOSED_SHELL('',*,#4905,.F.);
#216=ORIENTED_CLOSED_SHELL('',*,#4933,.F.);
#217=ORIENTED_CLOSED_SHELL('',*,#4934,.F.);
#218=BREP_WITH_VOIDS('Body1',#4906,(#215));
#219=BREP_WITH_VOIDS('Body1',#4932,(#216));
#220=BREP_WITH_VOIDS('Body1',#4935,(#217));
#221=B_SPLINE_CURVE_WITH_KNOTS('',3,(#9145,#9146,#9147,#9148,#9149,#9150,
#9151,#9152,#9153,#9154,#9155,#9156,#9157,#9158,#9159,#9160,#9161,#9162,
#9163,#9164,#9165,#9166,#9167,#9168,#9169,#9170,#9171,#9172,#9173,#9174,
#9175,#9176,#9177,#9178,#9179,#9180,#9181,#9182,#9183,#9184,#9185,#9186,
#9187,#9188,#9189,#9190,#9191,#9192,#9193,#9194,#9195,#9196,#9197,#9198,
#9199,#9200,#9201,#9202,#9203,#9204,#9205,#9206,#9207,#9208,#9209,#9210,
#9211,#9212,#9213,#9214,#9215,#9216,#9217,#9218,#9219,#9220,#9221,#9222,
#9223,#9224,#9225,#9226,#9227,#9228,#9229,#9230,#9231,#9232,#9233,#9234,
#9235,#9236,#9237,#9238,#9239,#9240,#9241,#9242,#9243,#9244,#9245,#9246,
#9247,#9248,#9249,#9250,#9251,#9252,#9253,#9254,#9255,#9256,#9257,#9258,
#9259,#9260,#9261,#9262,#9263,#9264,#9265,#9266),.UNSPECIFIED.,.F.,.F.,
(4,1,1,1,1,1,1,1,1,1,1,1,1,1,1,1,1,1,1,1,1,1,1,1,1,1,1,1,1,1,1,1,1,1,1,
1,1,1,1,1,1,1,1,1,1,1,1,1,1,1,1,1,1,1,1,1,1,1,1,1,1,1,1,1,1,1,1,1,1,1,1,
1,1,1,1,1,1,1,1,1,1,1,1,1,1,1,1,1,1,1,1,1,1,1,1,1,1,1,1,1,1,1,1,1,1,1,1,
1,1,1,1,1,1,1,1,1,1,1,1,4),(0.,0.00892857142857143,0.0178571428571429,0.0267857142857143,
0.0357142857142857,0.0446428571428571,0.0535714285714286,0.0625,0.0714285714285714,
0.0803571428571428,0.0892857142857143,0.0982142857142857,0.107142857142857,
0.116071428571429,0.120535714285714,0.125,0.129464285714286,0.133928571428571,
0.138392857142857,0.142857142857143,0.150793650793651,0.154761904761905,
0.158730158730159,0.166666666666667,0.174603174603175,0.17989417989418,
0.19047619047619,0.198412698412698,0.206349206349206,0.214285714285714,
0.222222222222222,0.227513227513228,0.238095238095238,0.25,0.261904761904762,
0.273809523809524,0.285714285714286,0.297619047619048,0.30952380952381,
0.321428571428571,0.333333333333333,0.341269841269841,0.349206349206349,
0.357142857142857,0.365079365079365,0.37037037037037,0.380952380952381,
0.386243386243386,0.396825396825397,0.404761904761905,0.412698412698413,
0.420634920634921,0.428571428571429,0.44047619047619,0.452380952380952,
0.458333333333333,0.464285714285714,0.470238095238095,0.476190476190476,
0.484126984126984,0.492063492063492,0.5,0.502232142857143,0.504464285714286,
0.508928571428571,0.517857142857143,0.526785714285714,0.535714285714286,
0.544642857142857,0.553571428571429,0.5625,0.571428571428571,0.580357142857143,
0.589285714285714,0.598214285714286,0.607142857142857,0.616071428571429,
0.625,0.633928571428571,0.642857142857143,0.650793650793651,0.658730158730159,
0.666666666666667,0.678571428571428,0.69047619047619,0.702380952380952,
0.714285714285714,0.726190476190476,0.738095238095238,0.746031746031746,
0.753968253968254,0.761904761904762,0.76984126984127,0.777777777777778,
0.785714285714286,0.790178571428571,0.794642857142857,0.803571428571428,
0.8125,0.821428571428571,0.830357142857143,0.839285714285714,0.848214285714286,
0.857142857142857,0.866071428571429,0.875,0.883928571428571,0.892857142857143,
0.901785714285714,0.910714285714286,0.919642857142857,0.928571428571429,
0.9375,0.946428571428571,0.955357142857143,0.964285714285714,0.973214285714286,
0.982142857142857,0.991071428571429,1.),.UNSPECIFIED.);
#222=B_SPLINE_CURVE_WITH_KNOTS('',3,(#9779,#9780,#9781,#9782,#9783,#9784,
#9785,#9786,#9787,#9788,#9789,#9790,#9791,#9792,#9793,#9794,#9795,#9796,
#9797,#9798,#9799,#9800),.UNSPECIFIED.,.F.,.F.,(4,2,2,2,2,2,2,2,2,2,4),
(0.0473477652366656,0.126350602536658,0.189525903804987,0.252701205073317,
0.313298422430275,0.373895639787233,0.434492857144191,0.495090074501149,
0.558265375769478,0.621440677037807,0.7004435143378),.UNSPECIFIED.);
#223=B_SPLINE_CURVE_WITH_KNOTS('',3,(#9804,#9805,#9806,#9807,#9808,#9809,
#9810,#9811,#9812,#9813,#9814,#9815,#9816,#9817,#9818,#9819,#9820,#9821,
#9822,#9823,#9824,#9825),.UNSPECIFIED.,.F.,.F.,(4,2,2,2,2,2,2,2,2,2,4),
(0.0464897534940957,0.0852567806515119,0.170513561303024,0.246687263103517,
0.308657850341199,0.370628437578881,0.432599024816563,0.494569612054245,
0.570743313854739,0.656000094506251,0.694767121663666),.UNSPECIFIED.);
#224=B_SPLINE_CURVE_WITH_KNOTS('',3,(#9831,#9832,#9833,#9834,#9835,#9836,
#9837,#9838,#9839,#9840,#9841,#9842,#9843,#9844,#9845,#9846,#9847,#9848,
#9849,#9850,#9851,#9852),.UNSPECIFIED.,.F.,.F.,(4,2,2,2,2,2,2,2,2,2,4),
(0.0464897534940957,0.0852567806515118,0.170513561303024,0.246687263103517,
0.308657850341199,0.370628437578881,0.432599024816563,0.494569612054245,
0.570743313854738,0.65600009450625,0.694767121663666),.UNSPECIFIED.);
#225=B_SPLINE_CURVE_WITH_KNOTS('',3,(#9856,#9857,#9858,#9859,#9860,#9861,
#9862,#9863,#9864,#9865,#9866,#9867,#9868,#9869,#9870,#9871,#9872,#9873,
#9874,#9875,#9876,#9877),.UNSPECIFIED.,.F.,.F.,(4,2,2,2,2,2,2,2,2,2,4),
(0.0464897534940957,0.0852567806515119,0.170513561303024,0.246687263103517,
0.308657850341199,0.370628437578881,0.432599024816563,0.494569612054245,
0.570743313854739,0.656000094506251,0.694767121663666),.UNSPECIFIED.);
#226=B_SPLINE_CURVE_WITH_KNOTS('',3,(#9881,#9882,#9883,#9884,#9885,#9886,
#9887,#9888,#9889,#9890,#9891,#9892),.UNSPECIFIED.,.F.,.F.,(4,2,2,2,2,4),
(0.0464897534940957,0.0852567806515119,0.170513561303024,0.246687263103517,
0.308657850341199,0.370628437578881),.UNSPECIFIED.);
#227=B_SPLINE_CURVE_WITH_KNOTS('',3,(#9897,#9898,#9899,#9900,#9901,#9902,
#9903,#9904,#9905,#9906,#9907,#9908),.UNSPECIFIED.,.F.,.F.,(4,2,2,2,2,4),
(0.370628437578881,0.432599024816563,0.494569612054245,0.570743313854738,
0.65600009450625,0.694767121663666),.UNSPECIFIED.);
#228=B_SPLINE_CURVE_WITH_KNOTS('',3,(#9912,#9913,#9914,#9915,#9916,#9917,
#9918,#9919,#9920,#9921,#9922,#9923,#9924,#9925,#9926,#9927,#9928,#9929,
#9930,#9931,#9932,#9933),.UNSPECIFIED.,.F.,.F.,(4,2,2,2,2,2,2,2,2,2,4),
(0.0464897534940957,0.0852567806515121,0.170513561303024,0.246687263103518,
0.308657850341199,0.370628437578881,0.432599024816563,0.494569612054245,
0.570743313854738,0.65600009450625,0.694767121663666),.UNSPECIFIED.);
#229=B_SPLINE_CURVE_WITH_KNOTS('',3,(#9937,#9938,#9939,#9940,#9941,#9942,
#9943,#9944,#9945,#9946,#9947,#9948,#9949,#9950,#9951,#9952,#9953,#9954,
#9955,#9956,#9957,#9958),.UNSPECIFIED.,.F.,.F.,(4,2,2,2,2,2,2,2,2,2,4),
(0.0464897534940957,0.0852567806515119,0.170513561303024,0.246687263103517,
0.308657850341199,0.370628437578881,0.432599024816563,0.494569612054245,
0.570743313854738,0.65600009450625,0.694767121663667),.UNSPECIFIED.);
#230=B_SPLINE_CURVE_WITH_KNOTS('',3,(#9962,#9963,#9964,#9965,#9966,#9967,
#9968,#9969,#9970,#9971,#9972,#9973,#9974,#9975,#9976,#9977,#9978,#9979,
#9980,#9981,#9982,#9983),.UNSPECIFIED.,.F.,.F.,(4,2,2,2,2,2,2,2,2,2,4),
(0.0464897534940957,0.0852567806515119,0.170513561303024,0.246687263103517,
0.308657850341199,0.370628437578881,0.432599024816563,0.494569612054245,
0.570743313854738,0.65600009450625,0.694767121663666),.UNSPECIFIED.);
#231=B_SPLINE_CURVE_WITH_KNOTS('',3,(#9987,#9988,#9989,#9990,#9991,#9992,
#9993,#9994,#9995,#9996,#9997,#9998,#9999,#10000,#10001,#10002,#10003,#10004,
#10005,#10006,#10007,#10008),.UNSPECIFIED.,.F.,.F.,(4,2,2,2,2,2,2,2,2,2,
4),(0.0464897534940957,0.0852567806515119,0.170513561303024,0.246687263103517,
0.308657850341199,0.370628437578881,0.432599024816563,0.494569612054245,
0.570743313854739,0.656000094506251,0.694767121663667),.UNSPECIFIED.);
#232=B_SPLINE_CURVE_WITH_KNOTS('',3,(#10016,#10017,#10018,#10019,#10020,
#10021,#10022,#10023,#10024,#10025,#10026,#10027,#10028,#10029,#10030,#10031,
#10032,#10033,#10034,#10035,#10036,#10037),.UNSPECIFIED.,.F.,.F.,(4,2,2,
2,2,2,2,2,2,2,4),(0.0473477652366656,0.126350602536658,0.189525903804987,
0.252701205073316,0.313298422430274,0.373895639787232,0.434492857144191,
0.495090074501149,0.558265375769478,0.621440677037807,0.7004435143378),
 .UNSPECIFIED.);
#233=B_SPLINE_CURVE_WITH_KNOTS('',3,(#10045,#10046,#10047,#10048,#10049,
#10050,#10051,#10052,#10053,#10054,#10055,#10056,#10057,#10058,#10059,#10060,
#10061,#10062,#10063,#10064,#10065,#10066),.UNSPECIFIED.,.F.,.F.,(4,2,2,
2,2,2,2,2,2,2,4),(0.0473477652366656,0.126350602536658,0.189525903804987,
0.252701205073317,0.313298422430275,0.373895639787233,0.434492857144191,
0.495090074501149,0.558265375769478,0.621440677037807,0.7004435143378),
 .UNSPECIFIED.);
#234=B_SPLINE_CURVE_WITH_KNOTS('',3,(#10075,#10076,#10077,#10078,#10079,
#10080,#10081,#10082,#10083,#10084,#10085,#10086),.UNSPECIFIED.,.F.,.F.,
(4,2,2,2,2,4),(0.0473477652366656,0.126350602536658,0.189525903804987,0.252701205073316,
0.313298422430275,0.373895639787233),.UNSPECIFIED.);
#235=B_SPLINE_CURVE_WITH_KNOTS('',3,(#10088,#10089,#10090,#10091,#10092,
#10093,#10094,#10095,#10096,#10097,#10098,#10099),.UNSPECIFIED.,.F.,.F.,
(4,2,2,2,2,4),(0.373895639787233,0.434492857144191,0.495090074501149,0.558265375769478,
0.621440677037807,0.7004435143378),.UNSPECIFIED.);
#236=B_SPLINE_CURVE_WITH_KNOTS('',3,(#10106,#10107,#10108,#10109,#10110,
#10111,#10112,#10113,#10114,#10115,#10116,#10117,#10118,#10119,#10120,#10121,
#10122,#10123,#10124,#10125,#10126,#10127),.UNSPECIFIED.,.F.,.F.,(4,2,2,
2,2,2,2,2,2,2,4),(0.0473477652366656,0.126350602536658,0.189525903804987,
0.252701205073316,0.313298422430275,0.373895639787233,0.434492857144191,
0.495090074501149,0.558265375769478,0.621440677037807,0.7004435143378),
 .UNSPECIFIED.);
#237=B_SPLINE_CURVE_WITH_KNOTS('',3,(#10135,#10136,#10137,#10138,#10139,
#10140,#10141,#10142,#10143,#10144,#10145,#10146,#10147,#10148,#10149,#10150,
#10151,#10152,#10153,#10154,#10155,#10156),.UNSPECIFIED.,.F.,.F.,(4,2,2,
2,2,2,2,2,2,2,4),(0.0473477652366656,0.126350602536658,0.189525903804987,
0.252701205073317,0.313298422430275,0.373895639787233,0.434492857144191,
0.495090074501149,0.558265375769478,0.621440677037807,0.7004435143378),
 .UNSPECIFIED.);
#238=B_SPLINE_CURVE_WITH_KNOTS('',3,(#10164,#10165,#10166,#10167,#10168,
#10169,#10170,#10171,#10172,#10173,#10174,#10175,#10176,#10177,#10178,#10179,
#10180,#10181,#10182,#10183,#10184,#10185),.UNSPECIFIED.,.F.,.F.,(4,2,2,
2,2,2,2,2,2,2,4),(0.0473477652366656,0.126350602536658,0.189525903804987,
0.252701205073316,0.313298422430275,0.373895639787233,0.434492857144191,
0.495090074501149,0.558265375769478,0.621440677037807,0.7004435143378),
 .UNSPECIFIED.);
#239=B_SPLINE_CURVE_WITH_KNOTS('',3,(#10194,#10195,#10196,#10197,#10198,
#10199,#10200,#10201,#10202,#10203,#10204,#10205,#10206,#10207,#10208,#10209,
#10210,#10211,#10212,#10213,#10214,#10215),.UNSPECIFIED.,.F.,.F.,(4,2,2,
2,2,2,2,2,2,2,4),(0.0473477652366656,0.126350602536658,0.189525903804987,
0.252701205073317,0.313298422430275,0.373895639787233,0.434492857144191,
0.495090074501149,0.558265375769478,0.621440677037807,0.7004435143378),
 .UNSPECIFIED.);
#240=B_SPLINE_SURFACE_WITH_KNOTS('',3,3,((#7922,#7923,#7924,#7925,#7926,
#7927,#7928,#7929,#7930,#7931,#7932,#7933,#7934,#7935,#7936,#7937,#7938,
#7939,#7940,#7941,#7942,#7943,#7944,#7945,#7946,#7947,#7948,#7949,#7950,
#7951,#7952,#7953,#7954,#7955,#7956,#7957,#7958,#7959,#7960,#7961,#7962,
#7963,#7964,#7965,#7966,#7967,#7968,#7969,#7970,#7971,#7972,#7973,#7974,
#7975,#7976,#7977,#7978,#7979,#7980,#7981,#7982,#7983,#7984,#7985,#7986,
#7987,#7988,#7989,#7990,#7991,#7992,#7993,#7994,#7995,#7996,#7997,#7998,
#7999,#8000,#8001,#8002,#8003,#8004,#8005,#8006,#8007,#8008,#8009,#8010,
#8011,#8012,#8013,#8014,#8015,#8016,#8017,#8018,#8019,#8020,#8021,#8022,
#8023,#8024,#8025,#8026,#8027,#8028,#8029,#8030,#8031,#8032,#8033,#8034,
#8035,#8036,#8037,#8038,#8039,#8040,#8041,#8042,#8043),(#8044,#8045,#8046,
#8047,#8048,#8049,#8050,#8051,#8052,#8053,#8054,#8055,#8056,#8057,#8058,
#8059,#8060,#8061,#8062,#8063,#8064,#8065,#8066,#8067,#8068,#8069,#8070,
#8071,#8072,#8073,#8074,#8075,#8076,#8077,#8078,#8079,#8080,#8081,#8082,
#8083,#8084,#8085,#8086,#8087,#8088,#8089,#8090,#8091,#8092,#8093,#8094,
#8095,#8096,#8097,#8098,#8099,#8100,#8101,#8102,#8103,#8104,#8105,#8106,
#8107,#8108,#8109,#8110,#8111,#8112,#8113,#8114,#8115,#8116,#8117,#8118,
#8119,#8120,#8121,#8122,#8123,#8124,#8125,#8126,#8127,#8128,#8129,#8130,
#8131,#8132,#8133,#8134,#8135,#8136,#8137,#8138,#8139,#8140,#8141,#8142,
#8143,#8144,#8145,#8146,#8147,#8148,#8149,#8150,#8151,#8152,#8153,#8154,
#8155,#8156,#8157,#8158,#8159,#8160,#8161,#8162,#8163,#8164,#8165),(#8166,
#8167,#8168,#8169,#8170,#8171,#8172,#8173,#8174,#8175,#8176,#8177,#8178,
#8179,#8180,#8181,#8182,#8183,#8184,#8185,#8186,#8187,#8188,#8189,#8190,
#8191,#8192,#8193,#8194,#8195,#8196,#8197,#8198,#8199,#8200,#8201,#8202,
#8203,#8204,#8205,#8206,#8207,#8208,#8209,#8210,#8211,#8212,#8213,#8214,
#8215,#8216,#8217,#8218,#8219,#8220,#8221,#8222,#8223,#8224,#8225,#8226,
#8227,#8228,#8229,#8230,#8231,#8232,#8233,#8234,#8235,#8236,#8237,#8238,
#8239,#8240,#8241,#8242,#8243,#8244,#8245,#8246,#8247,#8248,#8249,#8250,
#8251,#8252,#8253,#8254,#8255,#8256,#8257,#8258,#8259,#8260,#8261,#8262,
#8263,#8264,#8265,#8266,#8267,#8268,#8269,#8270,#8271,#8272,#8273,#8274,
#8275,#8276,#8277,#8278,#8279,#8280,#8281,#8282,#8283,#8284,#8285,#8286,
#8287),(#8288,#8289,#8290,#8291,#8292,#8293,#8294,#8295,#8296,#8297,#8298,
#8299,#8300,#8301,#8302,#8303,#8304,#8305,#8306,#8307,#8308,#8309,#8310,
#8311,#8312,#8313,#8314,#8315,#8316,#8317,#8318,#8319,#8320,#8321,#8322,
#8323,#8324,#8325,#8326,#8327,#8328,#8329,#8330,#8331,#8332,#8333,#8334,
#8335,#8336,#8337,#8338,#8339,#8340,#8341,#8342,#8343,#8344,#8345,#8346,
#8347,#8348,#8349,#8350,#8351,#8352,#8353,#8354,#8355,#8356,#8357,#8358,
#8359,#8360,#8361,#8362,#8363,#8364,#8365,#8366,#8367,#8368,#8369,#8370,
#8371,#8372,#8373,#8374,#8375,#8376,#8377,#8378,#8379,#8380,#8381,#8382,
#8383,#8384,#8385,#8386,#8387,#8388,#8389,#8390,#8391,#8392,#8393,#8394,
#8395,#8396,#8397,#8398,#8399,#8400,#8401,#8402,#8403,#8404,#8405,#8406,
#8407,#8408,#8409),(#8410,#8411,#8412,#8413,#8414,#8415,#8416,#8417,#8418,
#8419,#8420,#8421,#8422,#8423,#8424,#8425,#8426,#8427,#8428,#8429,#8430,
#8431,#8432,#8433,#8434,#8435,#8436,#8437,#8438,#8439,#8440,#8441,#8442,
#8443,#8444,#8445,#8446,#8447,#8448,#8449,#8450,#8451,#8452,#8453,#8454,
#8455,#8456,#8457,#8458,#8459,#8460,#8461,#8462,#8463,#8464,#8465,#8466,
#8467,#8468,#8469,#8470,#8471,#8472,#8473,#8474,#8475,#8476,#8477,#8478,
#8479,#8480,#8481,#8482,#8483,#8484,#8485,#8486,#8487,#8488,#8489,#8490,
#8491,#8492,#8493,#8494,#8495,#8496,#8497,#8498,#8499,#8500,#8501,#8502,
#8503,#8504,#8505,#8506,#8507,#8508,#8509,#8510,#8511,#8512,#8513,#8514,
#8515,#8516,#8517,#8518,#8519,#8520,#8521,#8522,#8523,#8524,#8525,#8526,
#8527,#8528,#8529,#8530,#8531),(#8532,#8533,#8534,#8535,#8536,#8537,#8538,
#8539,#8540,#8541,#8542,#8543,#8544,#8545,#8546,#8547,#8548,#8549,#8550,
#8551,#8552,#8553,#8554,#8555,#8556,#8557,#8558,#8559,#8560,#8561,#8562,
#8563,#8564,#8565,#8566,#8567,#8568,#8569,#8570,#8571,#8572,#8573,#8574,
#8575,#8576,#8577,#8578,#8579,#8580,#8581,#8582,#8583,#8584,#8585,#8586,
#8587,#8588,#8589,#8590,#8591,#8592,#8593,#8594,#8595,#8596,#8597,#8598,
#8599,#8600,#8601,#8602,#8603,#8604,#8605,#8606,#8607,#8608,#8609,#8610,
#8611,#8612,#8613,#8614,#8615,#8616,#8617,#8618,#8619,#8620,#8621,#8622,
#8623,#8624,#8625,#8626,#8627,#8628,#8629,#8630,#8631,#8632,#8633,#8634,
#8635,#8636,#8637,#8638,#8639,#8640,#8641,#8642,#8643,#8644,#8645,#8646,
#8647,#8648,#8649,#8650,#8651,#8652,#8653),(#8654,#8655,#8656,#8657,#8658,
#8659,#8660,#8661,#8662,#8663,#8664,#8665,#8666,#8667,#8668,#8669,#8670,
#8671,#8672,#8673,#8674,#8675,#8676,#8677,#8678,#8679,#8680,#8681,#8682,
#8683,#8684,#8685,#8686,#8687,#8688,#8689,#8690,#8691,#8692,#8693,#8694,
#8695,#8696,#8697,#8698,#8699,#8700,#8701,#8702,#8703,#8704,#8705,#8706,
#8707,#8708,#8709,#8710,#8711,#8712,#8713,#8714,#8715,#8716,#8717,#8718,
#8719,#8720,#8721,#8722,#8723,#8724,#8725,#8726,#8727,#8728,#8729,#8730,
#8731,#8732,#8733,#8734,#8735,#8736,#8737,#8738,#8739,#8740,#8741,#8742,
#8743,#8744,#8745,#8746,#8747,#8748,#8749,#8750,#8751,#8752,#8753,#8754,
#8755,#8756,#8757,#8758,#8759,#8760,#8761,#8762,#8763,#8764,#8765,#8766,
#8767,#8768,#8769,#8770,#8771,#8772,#8773,#8774,#8775),(#8776,#8777,#8778,
#8779,#8780,#8781,#8782,#8783,#8784,#8785,#8786,#8787,#8788,#8789,#8790,
#8791,#8792,#8793,#8794,#8795,#8796,#8797,#8798,#8799,#8800,#8801,#8802,
#8803,#8804,#8805,#8806,#8807,#8808,#8809,#8810,#8811,#8812,#8813,#8814,
#8815,#8816,#8817,#8818,#8819,#8820,#8821,#8822,#8823,#8824,#8825,#8826,
#8827,#8828,#8829,#8830,#8831,#8832,#8833,#8834,#8835,#8836,#8837,#8838,
#8839,#8840,#8841,#8842,#8843,#8844,#8845,#8846,#8847,#8848,#8849,#8850,
#8851,#8852,#8853,#8854,#8855,#8856,#8857,#8858,#8859,#8860,#8861,#8862,
#8863,#8864,#8865,#8866,#8867,#8868,#8869,#8870,#8871,#8872,#8873,#8874,
#8875,#8876,#8877,#8878,#8879,#8880,#8881,#8882,#8883,#8884,#8885,#8886,
#8887,#8888,#8889,#8890,#8891,#8892,#8893,#8894,#8895,#8896,#8897),(#8898,
#8899,#8900,#8901,#8902,#8903,#8904,#8905,#8906,#8907,#8908,#8909,#8910,
#8911,#8912,#8913,#8914,#8915,#8916,#8917,#8918,#8919,#8920,#8921,#8922,
#8923,#8924,#8925,#8926,#8927,#8928,#8929,#8930,#8931,#8932,#8933,#8934,
#8935,#8936,#8937,#8938,#8939,#8940,#8941,#8942,#8943,#8944,#8945,#8946,
#8947,#8948,#8949,#8950,#8951,#8952,#8953,#8954,#8955,#8956,#8957,#8958,
#8959,#8960,#8961,#8962,#8963,#8964,#8965,#8966,#8967,#8968,#8969,#8970,
#8971,#8972,#8973,#8974,#8975,#8976,#8977,#8978,#8979,#8980,#8981,#8982,
#8983,#8984,#8985,#8986,#8987,#8988,#8989,#8990,#8991,#8992,#8993,#8994,
#8995,#8996,#8997,#8998,#8999,#9000,#9001,#9002,#9003,#9004,#9005,#9006,
#9007,#9008,#9009,#9010,#9011,#9012,#9013,#9014,#9015,#9016,#9017,#9018,
#9019),(#9020,#9021,#9022,#9023,#9024,#9025,#9026,#9027,#9028,#9029,#9030,
#9031,#9032,#9033,#9034,#9035,#9036,#9037,#9038,#9039,#9040,#9041,#9042,
#9043,#9044,#9045,#9046,#9047,#9048,#9049,#9050,#9051,#9052,#9053,#9054,
#9055,#9056,#9057,#9058,#9059,#9060,#9061,#9062,#9063,#9064,#9065,#9066,
#9067,#9068,#9069,#9070,#9071,#9072,#9073,#9074,#9075,#9076,#9077,#9078,
#9079,#9080,#9081,#9082,#9083,#9084,#9085,#9086,#9087,#9088,#9089,#9090,
#9091,#9092,#9093,#9094,#9095,#9096,#9097,#9098,#9099,#9100,#9101,#9102,
#9103,#9104,#9105,#9106,#9107,#9108,#9109,#9110,#9111,#9112,#9113,#9114,
#9115,#9116,#9117,#9118,#9119,#9120,#9121,#9122,#9123,#9124,#9125,#9126,
#9127,#9128,#9129,#9130,#9131,#9132,#9133,#9134,#9135,#9136,#9137,#9138,
#9139,#9140,#9141)),.UNSPECIFIED.,.T.,.F.,.F.,(4,1,1,1,1,1,1,4),(4,1,1,
1,1,1,1,1,1,1,1,1,1,1,1,1,1,1,1,1,1,1,1,1,1,1,1,1,1,1,1,1,1,1,1,1,1,1,1,
1,1,1,1,1,1,1,1,1,1,1,1,1,1,1,1,1,1,1,1,1,1,1,1,1,1,1,1,1,1,1,1,1,1,1,1,
1,1,1,1,1,1,1,1,1,1,1,1,1,1,1,1,1,1,1,1,1,1,1,1,1,1,1,1,1,1,1,1,1,1,1,1,
1,1,1,1,1,1,1,1,4),(-3.14159265358979,-2.24399475256414,-1.34639685153848,
-0.448798950512828,0.448798950512828,1.34639685153848,2.24399475256414,
3.14159265358979),(0.,0.00892857142857143,0.0178571428571429,0.0267857142857143,
0.0357142857142857,0.0446428571428571,0.0535714285714286,0.0625,0.0714285714285714,
0.0803571428571428,0.0892857142857143,0.0982142857142857,0.107142857142857,
0.116071428571429,0.120535714285714,0.125,0.129464285714286,0.133928571428571,
0.138392857142857,0.142857142857143,0.150793650793651,0.154761904761905,
0.158730158730159,0.166666666666667,0.174603174603175,0.17989417989418,
0.19047619047619,0.198412698412698,0.206349206349206,0.214285714285714,
0.222222222222222,0.227513227513228,0.238095238095238,0.25,0.261904761904762,
0.273809523809524,0.285714285714286,0.297619047619048,0.30952380952381,
0.321428571428571,0.333333333333333,0.341269841269841,0.349206349206349,
0.357142857142857,0.365079365079365,0.37037037037037,0.380952380952381,
0.386243386243386,0.396825396825397,0.404761904761905,0.412698412698413,
0.420634920634921,0.428571428571429,0.44047619047619,0.452380952380952,
0.458333333333333,0.464285714285714,0.470238095238095,0.476190476190476,
0.484126984126984,0.492063492063492,0.5,0.502232142857143,0.504464285714286,
0.508928571428571,0.517857142857143,0.526785714285714,0.535714285714286,
0.544642857142857,0.553571428571429,0.5625,0.571428571428571,0.580357142857143,
0.589285714285714,0.598214285714286,0.607142857142857,0.616071428571429,
0.625,0.633928571428571,0.642857142857143,0.650793650793651,0.658730158730159,
0.666666666666667,0.678571428571428,0.69047619047619,0.702380952380952,
0.714285714285714,0.726190476190476,0.738095238095238,0.746031746031746,
0.753968253968254,0.761904761904762,0.76984126984127,0.777777777777778,
0.785714285714286,0.790178571428571,0.794642857142857,0.803571428571428,
0.8125,0.821428571428571,0.830357142857143,0.839285714285714,0.848214285714286,
0.857142857142857,0.866071428571429,0.875,0.883928571428571,0.892857142857143,
0.901785714285714,0.910714285714286,0.919642857142857,0.928571428571429,
0.9375,0.946428571428571,0.955357142857143,0.964285714285714,0.973214285714286,
0.982142857142857,0.991071428571429,1.),.UNSPECIFIED.);
#241=SHAPE_REPRESENTATION_RELATIONSHIP('SRR','None',#10739,#267);
#242=SHAPE_REPRESENTATION_RELATIONSHIP('SRR','None',#10740,#268);
#243=SHAPE_REPRESENTATION_RELATIONSHIP('SRR','None',#10741,#269);
#244=SHAPE_REPRESENTATION_RELATIONSHIP('SRR','None',#10742,#270);
#245=SHAPE_REPRESENTATION_RELATIONSHIP('SRR','None',#10743,#271);
#246=SHAPE_REPRESENTATION_RELATIONSHIP('SRR','None',#10744,#272);
#247=SHAPE_REPRESENTATION_RELATIONSHIP('SRR','None',#10745,#273);
#248=SHAPE_REPRESENTATION_RELATIONSHIP('SRR','None',#10747,#274);
#249=SHAPE_REPRESENTATION_RELATIONSHIP('SRR','None',#10748,#275);
#250=SHAPE_REPRESENTATION_RELATIONSHIP('SRR','None',#10749,#276);
#251=SHAPE_REPRESENTATION_RELATIONSHIP('SRR','None',#10750,#277);
#252=SHAPE_REPRESENTATION_RELATIONSHIP('SRR','None',#10751,#278);
#253=SHAPE_REPRESENTATION_RELATIONSHIP('SRR','None',#10752,#279);
#254=SHAPE_REPRESENTATION_RELATIONSHIP('SRR','None',#10753,#280);
#255=SHAPE_REPRESENTATION_RELATIONSHIP('SRR','None',#10755,#281);
#256=SHAPE_REPRESENTATION_RELATIONSHIP('SRR','None',#10756,#282);
#257=SHAPE_REPRESENTATION_RELATIONSHIP('SRR','None',#10757,#283);
#258=SHAPE_REPRESENTATION_RELATIONSHIP('SRR','None',#10758,#284);
#259=SHAPE_REPRESENTATION_RELATIONSHIP('SRR','None',#10759,#285);
#260=SHAPE_REPRESENTATION_RELATIONSHIP('SRR','None',#10761,#286);
#261=SHAPE_REPRESENTATION_RELATIONSHIP('SRR','None',#10762,#287);
#262=SHAPE_REPRESENTATION_RELATIONSHIP('SRR','None',#10763,#288);
#263=SHAPE_REPRESENTATION_RELATIONSHIP('SRR','None',#10764,#289);
#264=SHAPE_REPRESENTATION_RELATIONSHIP('SRR','None',#10765,#290);
#265=SHAPE_REPRESENTATION_RELATIONSHIP('SRR','None',#10766,#291);
#266=SHAPE_REPRESENTATION_RELATIONSHIP('SRR','None',#10767,#292);
#267=ADVANCED_BREP_SHAPE_REPRESENTATION('',(#327),#10598);
#268=ADVANCED_BREP_SHAPE_REPRESENTATION('',(#328),#10599);
#269=ADVANCED_BREP_SHAPE_REPRESENTATION('',(#329),#10600);
#270=ADVANCED_BREP_SHAPE_REPRESENTATION('',(#330),#10601);
#271=ADVANCED_BREP_SHAPE_REPRESENTATION('',(#331),#10602);
#272=ADVANCED_BREP_SHAPE_REPRESENTATION('',(#332),#10603);
#273=ADVANCED_BREP_SHAPE_REPRESENTATION('',(#218),#10604);
#274=ADVANCED_BREP_SHAPE_REPRESENTATION('',(#333),#10606);
#275=ADVANCED_BREP_SHAPE_REPRESENTATION('',(#334),#10607);
#276=ADVANCED_BREP_SHAPE_REPRESENTATION('',(#335),#10608);
#277=ADVANCED_BREP_SHAPE_REPRESENTATION('',(#336),#10609);
#278=ADVANCED_BREP_SHAPE_REPRESENTATION('',(#337),#10610);
#279=ADVANCED_BREP_SHAPE_REPRESENTATION('',(#338),#10611);
#280=ADVANCED_BREP_SHAPE_REPRESENTATION('',(#339),#10612);
#281=ADVANCED_BREP_SHAPE_REPRESENTATION('',(#340),#10614);
#282=ADVANCED_BREP_SHAPE_REPRESENTATION('',(#341),#10615);
#283=ADVANCED_BREP_SHAPE_REPRESENTATION('',(#342,#343,#344,#345,#346,#347,
#348,#349),#10616);
#284=ADVANCED_BREP_SHAPE_REPRESENTATION('',(#350),#10617);
#285=ADVANCED_BREP_SHAPE_REPRESENTATION('',(#351,#352),#10618);
#286=ADVANCED_BREP_SHAPE_REPRESENTATION('',(#353),#10620);
#287=ADVANCED_BREP_SHAPE_REPRESENTATION('',(#354),#10621);
#288=ADVANCED_BREP_SHAPE_REPRESENTATION('',(#355),#10622);
#289=ADVANCED_BREP_SHAPE_REPRESENTATION('',(#356),#10623);
#290=ADVANCED_BREP_SHAPE_REPRESENTATION('',(#357),#10624);
#291=ADVANCED_BREP_SHAPE_REPRESENTATION('',(#219),#10625);
#292=ADVANCED_BREP_SHAPE_REPRESENTATION('',(#220),#10626);
#293=STYLED_ITEM('',(#10944),#327);
#294=STYLED_ITEM('',(#10951),#328);
#295=STYLED_ITEM('',(#10951),#329);
#296=STYLED_ITEM('',(#10958),#330);
#297=STYLED_ITEM('',(#10958),#331);
#298=STYLED_ITEM('',(#10965),#332);
#299=STYLED_ITEM('',(#10972),#218);
#300=STYLED_ITEM('',(#10965),#333);
#301=STYLED_ITEM('',(#10965),#334);
#302=STYLED_ITEM('',(#10965),#335);
#303=STYLED_ITEM('',(#10965),#336);
#304=STYLED_ITEM('',(#10951),#337);
#305=STYLED_ITEM('',(#10951),#338);
#306=STYLED_ITEM('',(#10958),#339);
#307=STYLED_ITEM('',(#10965),#340);
#308=STYLED_ITEM('',(#10965),#341);
#309=STYLED_ITEM('',(#10965),#342);
#310=STYLED_ITEM('',(#10965),#343);
#311=STYLED_ITEM('',(#10965),#344);
#312=STYLED_ITEM('',(#10965),#345);
#313=STYLED_ITEM('',(#10965),#346);
#314=STYLED_ITEM('',(#10965),#347);
#315=STYLED_ITEM('',(#10965),#348);
#316=STYLED_ITEM('',(#10965),#349);
#317=STYLED_ITEM('',(#10965),#350);
#318=STYLED_ITEM('',(#10965),#351);
#319=STYLED_ITEM('',(#10965),#352);
#320=STYLED_ITEM('',(#10965),#353);
#321=STYLED_ITEM('',(#10958),#354);
#322=STYLED_ITEM('',(#10972),#355);
#323=STYLED_ITEM('',(#10965),#356);
#324=STYLED_ITEM('',(#10965),#357);
#325=STYLED_ITEM('',(#10972),#219);
#326=STYLED_ITEM('',(#10972),#220);
#327=MANIFOLD_SOLID_BREP('Body1',#4899);
#328=MANIFOLD_SOLID_BREP('Body1',#4900);
#329=MANIFOLD_SOLID_BREP('Body1',#4901);
#330=MANIFOLD_SOLID_BREP('Body1',#4902);
#331=MANIFOLD_SOLID_BREP('Body1',#4903);
#332=MANIFOLD_SOLID_BREP('Body1',#4904);
#333=MANIFOLD_SOLID_BREP('Body1',#4907);
#334=MANIFOLD_SOLID_BREP('Body1',#4908);
#335=MANIFOLD_SOLID_BREP('Body1',#4909);
#336=MANIFOLD_SOLID_BREP('Body1',#4910);
#337=MANIFOLD_SOLID_BREP('Body1',#4911);
#338=MANIFOLD_SOLID_BREP('Body1',#4912);
#339=MANIFOLD_SOLID_BREP('Body1',#4913);
#340=MANIFOLD_SOLID_BREP('Body1',#4914);
#341=MANIFOLD_SOLID_BREP('Body1',#4915);
#342=MANIFOLD_SOLID_BREP('Body1',#4916);
#343=MANIFOLD_SOLID_BREP('Body2',#4917);
#344=MANIFOLD_SOLID_BREP('Body3',#4918);
#345=MANIFOLD_SOLID_BREP('Body4',#4919);
#346=MANIFOLD_SOLID_BREP('Body5',#4920);
#347=MANIFOLD_SOLID_BREP('Body6',#4921);
#348=MANIFOLD_SOLID_BREP('Body7',#4922);
#349=MANIFOLD_SOLID_BREP('Body8',#4923);
#350=MANIFOLD_SOLID_BREP('Continuous crown cage',#4924);
#351=MANIFOLD_SOLID_BREP('Body1',#4925);
#352=MANIFOLD_SOLID_BREP('Body2',#4926);
#353=MANIFOLD_SOLID_BREP('Body1',#4927);
#354=MANIFOLD_SOLID_BREP('Body1',#4928);
#355=MANIFOLD_SOLID_BREP('Body1',#4929);
#356=MANIFOLD_SOLID_BREP('Body1',#4930);
#357=MANIFOLD_SOLID_BREP('Body1',#4931);
#358=FACE_BOUND('',#953,.T.);
#359=FACE_BOUND('',#954,.T.);
#360=FACE_BOUND('',#955,.T.);
#361=FACE_BOUND('',#956,.T.);
#362=FACE_BOUND('',#958,.T.);
#363=FACE_BOUND('',#959,.T.);
#364=FACE_BOUND('',#960,.T.);
#365=FACE_BOUND('',#961,.T.);
#366=FACE_BOUND('',#975,.T.);
#367=FACE_BOUND('',#978,.T.);
#368=FACE_BOUND('',#981,.T.);
#369=FACE_BOUND('',#984,.T.);
#370=FACE_BOUND('',#987,.T.);
#371=FACE_BOUND('',#992,.T.);
#372=FACE_BOUND('',#1004,.T.);
#373=FACE_BOUND('',#1005,.T.);
#374=FACE_BOUND('',#1012,.T.);
#375=FACE_BOUND('',#1018,.T.);
#376=FACE_BOUND('',#1022,.T.);
#377=FACE_BOUND('',#1028,.T.);
#378=FACE_BOUND('',#1039,.T.);
#379=FACE_BOUND('',#1042,.T.);
#380=FACE_BOUND('',#1045,.T.);
#381=FACE_BOUND('',#1046,.T.);
#382=FACE_BOUND('',#1047,.T.);
#383=FACE_BOUND('',#1048,.T.);
#384=FACE_BOUND('',#1072,.T.);
#385=FACE_BOUND('',#1095,.T.);
#386=FACE_BOUND('',#1101,.T.);
#387=FACE_BOUND('',#1103,.T.);
#388=FACE_BOUND('',#1104,.T.);
#389=FACE_BOUND('',#1105,.T.);
#390=FACE_BOUND('',#1106,.T.);
#391=FACE_BOUND('',#1107,.T.);
#392=FACE_BOUND('',#1109,.T.);
#393=FACE_BOUND('',#1110,.T.);
#394=FACE_BOUND('',#1111,.T.);
#395=FACE_BOUND('',#1112,.T.);
#396=FACE_BOUND('',#1113,.T.);
#397=FACE_BOUND('',#1117,.T.);
#398=FACE_BOUND('',#1119,.T.);
#399=FACE_BOUND('',#1123,.T.);
#400=FACE_BOUND('',#1125,.T.);
#401=FACE_BOUND('',#1128,.T.);
#402=FACE_BOUND('',#1131,.T.);
#403=FACE_BOUND('',#1134,.T.);
#404=FACE_BOUND('',#1137,.T.);
#405=FACE_BOUND('',#1144,.T.);
#406=FACE_BOUND('',#1148,.T.);
#407=FACE_BOUND('',#1149,.T.);
#408=FACE_BOUND('',#1150,.T.);
#409=FACE_BOUND('',#1151,.T.);
#410=FACE_BOUND('',#1152,.T.);
#411=FACE_BOUND('',#1154,.T.);
#412=FACE_BOUND('',#1155,.T.);
#413=FACE_BOUND('',#1156,.T.);
#414=FACE_BOUND('',#1157,.T.);
#415=FACE_BOUND('',#1158,.T.);
#416=FACE_BOUND('',#1161,.T.);
#417=FACE_BOUND('',#1164,.T.);
#418=FACE_BOUND('',#1167,.T.);
#419=FACE_BOUND('',#1170,.T.);
#420=FACE_BOUND('',#1180,.T.);
#421=FACE_BOUND('',#1184,.T.);
#422=FACE_BOUND('',#1185,.T.);
#423=FACE_BOUND('',#1186,.T.);
#424=FACE_BOUND('',#1187,.T.);
#425=FACE_BOUND('',#1188,.T.);
#426=FACE_BOUND('',#1190,.T.);
#427=FACE_BOUND('',#1191,.T.);
#428=FACE_BOUND('',#1192,.T.);
#429=FACE_BOUND('',#1193,.T.);
#430=FACE_BOUND('',#1194,.T.);
#431=FACE_BOUND('',#1199,.T.);
#432=FACE_BOUND('',#1209,.T.);
#433=FACE_BOUND('',#1212,.T.);
#434=FACE_BOUND('',#1217,.T.);
#435=FACE_BOUND('',#1222,.T.);
#436=FACE_BOUND('',#1250,.T.);
#437=FACE_BOUND('',#1253,.T.);
#438=FACE_BOUND('',#1256,.T.);
#439=FACE_BOUND('',#1259,.T.);
#440=FACE_BOUND('',#1262,.T.);
#441=FACE_BOUND('',#1269,.T.);
#442=FACE_BOUND('',#1272,.T.);
#443=FACE_BOUND('',#1277,.T.);
#444=FACE_BOUND('',#1279,.T.);
#445=FACE_BOUND('',#1282,.T.);
#446=FACE_BOUND('',#1284,.T.);
#447=FACE_BOUND('',#1288,.T.);
#448=FACE_BOUND('',#1289,.T.);
#449=FACE_BOUND('',#1293,.T.);
#450=FACE_BOUND('',#1297,.T.);
#451=FACE_BOUND('',#1302,.T.);
#452=FACE_BOUND('',#1307,.T.);
#453=FACE_BOUND('',#1309,.T.);
#454=FACE_BOUND('',#1313,.T.);
#455=FACE_BOUND('',#1315,.T.);
#456=FACE_BOUND('',#1321,.T.);
#457=FACE_BOUND('',#1348,.T.);
#458=PLANE('',#5238);
#459=PLANE('',#5239);
#460=PLANE('',#5240);
#461=PLANE('',#5241);
#462=PLANE('',#5242);
#463=PLANE('',#5243);
#464=PLANE('',#5245);
#465=PLANE('',#5246);
#466=PLANE('',#5247);
#467=PLANE('',#5248);
#468=PLANE('',#5249);
#469=PLANE('',#5250);
#470=PLANE('',#5252);
#471=PLANE('',#5253);
#472=PLANE('',#5254);
#473=PLANE('',#5255);
#474=PLANE('',#5256);
#475=PLANE('',#5257);
#476=PLANE('',#5259);
#477=PLANE('',#5265);
#478=PLANE('',#5271);
#479=PLANE('',#5277);
#480=PLANE('',#5283);
#481=PLANE('',#5295);
#482=PLANE('',#5296);
#483=PLANE('',#5297);
#484=PLANE('',#5298);
#485=PLANE('',#5299);
#486=PLANE('',#5300);
#487=PLANE('',#5301);
#488=PLANE('',#5303);
#489=PLANE('',#5304);
#490=PLANE('',#5305);
#491=PLANE('',#5306);
#492=PLANE('',#5307);
#493=PLANE('',#5318);
#494=PLANE('',#5319);
#495=PLANE('',#5320);
#496=PLANE('',#5321);
#497=PLANE('',#5322);
#498=PLANE('',#5323);
#499=PLANE('',#5324);
#500=PLANE('',#5325);
#501=PLANE('',#5326);
#502=PLANE('',#5327);
#503=PLANE('',#5328);
#504=PLANE('',#5332);
#505=PLANE('',#5333);
#506=PLANE('',#5334);
#507=PLANE('',#5335);
#508=PLANE('',#5336);
#509=PLANE('',#5337);
#510=PLANE('',#5338);
#511=PLANE('',#5339);
#512=PLANE('',#5340);
#513=PLANE('',#5341);
#514=PLANE('',#5342);
#515=PLANE('',#5351);
#516=PLANE('',#5356);
#517=PLANE('',#5358);
#518=PLANE('',#5360);
#519=PLANE('',#5361);
#520=PLANE('',#5362);
#521=PLANE('',#5363);
#522=PLANE('',#5364);
#523=PLANE('',#5365);
#524=PLANE('',#5369);
#525=PLANE('',#5370);
#526=PLANE('',#5372);
#527=PLANE('',#5373);
#528=PLANE('',#5374);
#529=PLANE('',#5375);
#530=PLANE('',#5376);
#531=PLANE('',#5377);
#532=PLANE('',#5378);
#533=PLANE('',#5379);
#534=PLANE('',#5380);
#535=PLANE('',#5382);
#536=PLANE('',#5390);
#537=PLANE('',#5410);
#538=PLANE('',#5414);
#539=PLANE('',#5418);
#540=PLANE('',#5422);
#541=PLANE('',#5426);
#542=PLANE('',#5430);
#543=PLANE('',#5434);
#544=PLANE('',#5438);
#545=PLANE('',#5442);
#546=PLANE('',#5446);
#547=PLANE('',#5448);
#548=PLANE('',#5449);
#549=PLANE('',#5450);
#550=PLANE('',#5458);
#551=PLANE('',#5459);
#552=PLANE('',#5467);
#553=PLANE('',#5468);
#554=PLANE('',#5476);
#555=PLANE('',#5477);
#556=PLANE('',#5482);
#557=PLANE('',#5487);
#558=PLANE('',#5492);
#559=PLANE('',#5497);
#560=PLANE('',#5510);
#561=PLANE('',#5517);
#562=PLANE('',#5518);
#563=PLANE('',#5523);
#564=PLANE('',#5528);
#565=PLANE('',#5533);
#566=PLANE('',#5538);
#567=PLANE('',#5548);
#568=PLANE('',#5549);
#569=PLANE('',#5550);
#570=PLANE('',#5554);
#571=PLANE('',#5561);
#572=PLANE('',#5562);
#573=PLANE('',#5567);
#574=PLANE('',#5571);
#575=PLANE('',#5572);
#576=PLANE('',#5577);
#577=PLANE('',#5578);
#578=PLANE('',#5594);
#579=PLANE('',#5597);
#580=PLANE('',#5609);
#581=PLANE('',#5618);
#582=PLANE('',#5651);
#583=PLANE('',#5656);
#584=PLANE('',#5661);
#585=PLANE('',#5666);
#586=PLANE('',#5671);
#587=PLANE('',#5676);
#588=PLANE('',#5685);
#589=PLANE('',#5689);
#590=PLANE('',#5690);
#591=PLANE('',#5692);
#592=PLANE('',#5697);
#593=PLANE('',#5700);
#594=PLANE('',#5705);
#595=PLANE('',#5718);
#596=PLANE('',#5722);
#597=PLANE('',#5723);
#598=PLANE('',#5728);
#599=PLANE('',#5737);
#600=PLANE('',#5738);
#601=PLANE('',#5742);
#602=PLANE('',#5743);
#603=PLANE('',#5751);
#604=PLANE('',#5755);
#605=PLANE('',#5756);
#606=PLANE('',#5757);
#607=PLANE('',#5763);
#608=PLANE('',#5768);
#609=PLANE('',#5772);
#610=PLANE('',#5773);
#611=PLANE('',#5781);
#612=PLANE('',#5782);
#613=PLANE('',#5790);
#614=PLANE('',#5791);
#615=PLANE('',#5793);
#616=PLANE('',#5801);
#617=PLANE('',#5809);
#618=PLANE('',#5810);
#619=PLANE('',#5811);
#620=PLANE('',#5812);
#621=PLANE('',#5813);
#622=PLANE('',#5814);
#623=PLANE('',#5815);
#624=PLANE('',#5816);
#625=PLANE('',#5817);
#626=PLANE('',#5819);
#627=PLANE('',#5820);
#628=PLANE('',#5821);
#629=PLANE('',#5822);
#630=PLANE('',#5823);
#631=PLANE('',#5824);
#632=PLANE('',#5825);
#633=PLANE('',#5826);
#634=PLANE('',#5827);
#635=PLANE('',#5829);
#636=PLANE('',#5837);
#637=FACE_OUTER_BOUND('',#944,.T.);
#638=FACE_OUTER_BOUND('',#945,.T.);
#639=FACE_OUTER_BOUND('',#946,.T.);
#640=FACE_OUTER_BOUND('',#947,.T.);
#641=FACE_OUTER_BOUND('',#948,.T.);
#642=FACE_OUTER_BOUND('',#949,.T.);
#643=FACE_OUTER_BOUND('',#950,.T.);
#644=FACE_OUTER_BOUND('',#951,.T.);
#645=FACE_OUTER_BOUND('',#952,.T.);
#646=FACE_OUTER_BOUND('',#957,.T.);
#647=FACE_OUTER_BOUND('',#962,.T.);
#648=FACE_OUTER_BOUND('',#963,.T.);
#649=FACE_OUTER_BOUND('',#964,.T.);
#650=FACE_OUTER_BOUND('',#965,.T.);
#651=FACE_OUTER_BOUND('',#966,.T.);
#652=FACE_OUTER_BOUND('',#967,.T.);
#653=FACE_OUTER_BOUND('',#968,.T.);
#654=FACE_OUTER_BOUND('',#969,.T.);
#655=FACE_OUTER_BOUND('',#970,.T.);
#656=FACE_OUTER_BOUND('',#971,.T.);
#657=FACE_OUTER_BOUND('',#972,.T.);
#658=FACE_OUTER_BOUND('',#973,.T.);
#659=FACE_OUTER_BOUND('',#974,.T.);
#660=FACE_OUTER_BOUND('',#976,.T.);
#661=FACE_OUTER_BOUND('',#977,.T.);
#662=FACE_OUTER_BOUND('',#979,.T.);
#663=FACE_OUTER_BOUND('',#980,.T.);
#664=FACE_OUTER_BOUND('',#982,.T.);
#665=FACE_OUTER_BOUND('',#983,.T.);
#666=FACE_OUTER_BOUND('',#985,.T.);
#667=FACE_OUTER_BOUND('',#986,.T.);
#668=FACE_OUTER_BOUND('',#988,.T.);
#669=FACE_OUTER_BOUND('',#989,.T.);
#670=FACE_OUTER_BOUND('',#990,.T.);
#671=FACE_OUTER_BOUND('',#991,.T.);
#672=FACE_OUTER_BOUND('',#993,.T.);
#673=FACE_OUTER_BOUND('',#994,.T.);
#674=FACE_OUTER_BOUND('',#995,.T.);
#675=FACE_OUTER_BOUND('',#996,.T.);
#676=FACE_OUTER_BOUND('',#997,.T.);
#677=FACE_OUTER_BOUND('',#998,.T.);
#678=FACE_OUTER_BOUND('',#999,.T.);
#679=FACE_OUTER_BOUND('',#1000,.T.);
#680=FACE_OUTER_BOUND('',#1001,.T.);
#681=FACE_OUTER_BOUND('',#1002,.T.);
#682=FACE_OUTER_BOUND('',#1003,.T.);
#683=FACE_OUTER_BOUND('',#1006,.T.);
#684=FACE_OUTER_BOUND('',#1007,.T.);
#685=FACE_OUTER_BOUND('',#1008,.T.);
#686=FACE_OUTER_BOUND('',#1009,.T.);
#687=FACE_OUTER_BOUND('',#1010,.T.);
#688=FACE_OUTER_BOUND('',#1011,.T.);
#689=FACE_OUTER_BOUND('',#1013,.T.);
#690=FACE_OUTER_BOUND('',#1014,.T.);
#691=FACE_OUTER_BOUND('',#1015,.T.);
#692=FACE_OUTER_BOUND('',#1016,.T.);
#693=FACE_OUTER_BOUND('',#1017,.T.);
#694=FACE_OUTER_BOUND('',#1019,.T.);
#695=FACE_OUTER_BOUND('',#1020,.T.);
#696=FACE_OUTER_BOUND('',#1021,.T.);
#697=FACE_OUTER_BOUND('',#1023,.T.);
#698=FACE_OUTER_BOUND('',#1024,.T.);
#699=FACE_OUTER_BOUND('',#1025,.T.);
#700=FACE_OUTER_BOUND('',#1026,.T.);
#701=FACE_OUTER_BOUND('',#1027,.T.);
#702=FACE_OUTER_BOUND('',#1029,.T.);
#703=FACE_OUTER_BOUND('',#1030,.T.);
#704=FACE_OUTER_BOUND('',#1031,.T.);
#705=FACE_OUTER_BOUND('',#1032,.T.);
#706=FACE_OUTER_BOUND('',#1033,.T.);
#707=FACE_OUTER_BOUND('',#1034,.T.);
#708=FACE_OUTER_BOUND('',#1035,.T.);
#709=FACE_OUTER_BOUND('',#1036,.T.);
#710=FACE_OUTER_BOUND('',#1037,.T.);
#711=FACE_OUTER_BOUND('',#1038,.T.);
#712=FACE_OUTER_BOUND('',#1040,.T.);
#713=FACE_OUTER_BOUND('',#1041,.T.);
#714=FACE_OUTER_BOUND('',#1043,.T.);
#715=FACE_OUTER_BOUND('',#1044,.T.);
#716=FACE_OUTER_BOUND('',#1049,.T.);
#717=FACE_OUTER_BOUND('',#1050,.T.);
#718=FACE_OUTER_BOUND('',#1051,.T.);
#719=FACE_OUTER_BOUND('',#1052,.T.);
#720=FACE_OUTER_BOUND('',#1053,.T.);
#721=FACE_OUTER_BOUND('',#1054,.T.);
#722=FACE_OUTER_BOUND('',#1055,.T.);
#723=FACE_OUTER_BOUND('',#1056,.T.);
#724=FACE_OUTER_BOUND('',#1057,.T.);
#725=FACE_OUTER_BOUND('',#1058,.T.);
#726=FACE_OUTER_BOUND('',#1059,.T.);
#727=FACE_OUTER_BOUND('',#1060,.T.);
#728=FACE_OUTER_BOUND('',#1061,.T.);
#729=FACE_OUTER_BOUND('',#1062,.T.);
#730=FACE_OUTER_BOUND('',#1063,.T.);
#731=FACE_OUTER_BOUND('',#1064,.T.);
#732=FACE_OUTER_BOUND('',#1065,.T.);
#733=FACE_OUTER_BOUND('',#1066,.T.);
#734=FACE_OUTER_BOUND('',#1067,.T.);
#735=FACE_OUTER_BOUND('',#1068,.T.);
#736=FACE_OUTER_BOUND('',#1069,.T.);
#737=FACE_OUTER_BOUND('',#1070,.T.);
#738=FACE_OUTER_BOUND('',#1071,.T.);
#739=FACE_OUTER_BOUND('',#1073,.T.);
#740=FACE_OUTER_BOUND('',#1074,.T.);
#741=FACE_OUTER_BOUND('',#1075,.T.);
#742=FACE_OUTER_BOUND('',#1076,.T.);
#743=FACE_OUTER_BOUND('',#1077,.T.);
#744=FACE_OUTER_BOUND('',#1078,.T.);
#745=FACE_OUTER_BOUND('',#1079,.T.);
#746=FACE_OUTER_BOUND('',#1080,.T.);
#747=FACE_OUTER_BOUND('',#1081,.T.);
#748=FACE_OUTER_BOUND('',#1082,.T.);
#749=FACE_OUTER_BOUND('',#1083,.T.);
#750=FACE_OUTER_BOUND('',#1084,.T.);
#751=FACE_OUTER_BOUND('',#1085,.T.);
#752=FACE_OUTER_BOUND('',#1086,.T.);
#753=FACE_OUTER_BOUND('',#1087,.T.);
#754=FACE_OUTER_BOUND('',#1088,.T.);
#755=FACE_OUTER_BOUND('',#1089,.T.);
#756=FACE_OUTER_BOUND('',#1090,.T.);
#757=FACE_OUTER_BOUND('',#1091,.T.);
#758=FACE_OUTER_BOUND('',#1092,.T.);
#759=FACE_OUTER_BOUND('',#1093,.T.);
#760=FACE_OUTER_BOUND('',#1094,.T.);
#761=FACE_OUTER_BOUND('',#1096,.T.);
#762=FACE_OUTER_BOUND('',#1097,.T.);
#763=FACE_OUTER_BOUND('',#1098,.T.);
#764=FACE_OUTER_BOUND('',#1099,.T.);
#765=FACE_OUTER_BOUND('',#1100,.T.);
#766=FACE_OUTER_BOUND('',#1102,.T.);
#767=FACE_OUTER_BOUND('',#1108,.T.);
#768=FACE_OUTER_BOUND('',#1114,.T.);
#769=FACE_OUTER_BOUND('',#1115,.T.);
#770=FACE_OUTER_BOUND('',#1116,.T.);
#771=FACE_OUTER_BOUND('',#1118,.T.);
#772=FACE_OUTER_BOUND('',#1120,.T.);
#773=FACE_OUTER_BOUND('',#1121,.T.);
#774=FACE_OUTER_BOUND('',#1122,.T.);
#775=FACE_OUTER_BOUND('',#1124,.T.);
#776=FACE_OUTER_BOUND('',#1126,.T.);
#777=FACE_OUTER_BOUND('',#1127,.T.);
#778=FACE_OUTER_BOUND('',#1129,.T.);
#779=FACE_OUTER_BOUND('',#1130,.T.);
#780=FACE_OUTER_BOUND('',#1132,.T.);
#781=FACE_OUTER_BOUND('',#1133,.T.);
#782=FACE_OUTER_BOUND('',#1135,.T.);
#783=FACE_OUTER_BOUND('',#1136,.T.);
#784=FACE_OUTER_BOUND('',#1138,.T.);
#785=FACE_OUTER_BOUND('',#1139,.T.);
#786=FACE_OUTER_BOUND('',#1140,.T.);
#787=FACE_OUTER_BOUND('',#1141,.T.);
#788=FACE_OUTER_BOUND('',#1142,.T.);
#789=FACE_OUTER_BOUND('',#1143,.T.);
#790=FACE_OUTER_BOUND('',#1145,.T.);
#791=FACE_OUTER_BOUND('',#1146,.T.);
#792=FACE_OUTER_BOUND('',#1147,.T.);
#793=FACE_OUTER_BOUND('',#1153,.T.);
#794=FACE_OUTER_BOUND('',#1159,.T.);
#795=FACE_OUTER_BOUND('',#1160,.T.);
#796=FACE_OUTER_BOUND('',#1162,.T.);
#797=FACE_OUTER_BOUND('',#1163,.T.);
#798=FACE_OUTER_BOUND('',#1165,.T.);
#799=FACE_OUTER_BOUND('',#1166,.T.);
#800=FACE_OUTER_BOUND('',#1168,.T.);
#801=FACE_OUTER_BOUND('',#1169,.T.);
#802=FACE_OUTER_BOUND('',#1171,.T.);
#803=FACE_OUTER_BOUND('',#1172,.T.);
#804=FACE_OUTER_BOUND('',#1173,.T.);
#805=FACE_OUTER_BOUND('',#1174,.T.);
#806=FACE_OUTER_BOUND('',#1175,.T.);
#807=FACE_OUTER_BOUND('',#1176,.T.);
#808=FACE_OUTER_BOUND('',#1177,.T.);
#809=FACE_OUTER_BOUND('',#1178,.T.);
#810=FACE_OUTER_BOUND('',#1179,.T.);
#811=FACE_OUTER_BOUND('',#1181,.T.);
#812=FACE_OUTER_BOUND('',#1182,.T.);
#813=FACE_OUTER_BOUND('',#1183,.T.);
#814=FACE_OUTER_BOUND('',#1189,.T.);
#815=FACE_OUTER_BOUND('',#1195,.T.);
#816=FACE_OUTER_BOUND('',#1196,.T.);
#817=FACE_OUTER_BOUND('',#1197,.T.);
#818=FACE_OUTER_BOUND('',#1198,.T.);
#819=FACE_OUTER_BOUND('',#1200,.T.);
#820=FACE_OUTER_BOUND('',#1201,.T.);
#821=FACE_OUTER_BOUND('',#1202,.T.);
#822=FACE_OUTER_BOUND('',#1203,.T.);
#823=FACE_OUTER_BOUND('',#1204,.T.);
#824=FACE_OUTER_BOUND('',#1205,.T.);
#825=FACE_OUTER_BOUND('',#1206,.T.);
#826=FACE_OUTER_BOUND('',#1207,.T.);
#827=FACE_OUTER_BOUND('',#1208,.T.);
#828=FACE_OUTER_BOUND('',#1210,.T.);
#829=FACE_OUTER_BOUND('',#1211,.T.);
#830=FACE_OUTER_BOUND('',#1213,.T.);
#831=FACE_OUTER_BOUND('',#1214,.T.);
#832=FACE_OUTER_BOUND('',#1215,.T.);
#833=FACE_OUTER_BOUND('',#1216,.T.);
#834=FACE_OUTER_BOUND('',#1218,.T.);
#835=FACE_OUTER_BOUND('',#1219,.T.);
#836=FACE_OUTER_BOUND('',#1220,.T.);
#837=FACE_OUTER_BOUND('',#1221,.T.);
#838=FACE_OUTER_BOUND('',#1223,.T.);
#839=FACE_OUTER_BOUND('',#1224,.T.);
#840=FACE_OUTER_BOUND('',#1225,.T.);
#841=FACE_OUTER_BOUND('',#1226,.T.);
#842=FACE_OUTER_BOUND('',#1227,.T.);
#843=FACE_OUTER_BOUND('',#1228,.T.);
#844=FACE_OUTER_BOUND('',#1229,.T.);
#845=FACE_OUTER_BOUND('',#1230,.T.);
#846=FACE_OUTER_BOUND('',#1231,.T.);
#847=FACE_OUTER_BOUND('',#1232,.T.);
#848=FACE_OUTER_BOUND('',#1233,.T.);
#849=FACE_OUTER_BOUND('',#1234,.T.);
#850=FACE_OUTER_BOUND('',#1235,.T.);
#851=FACE_OUTER_BOUND('',#1236,.T.);
#852=FACE_OUTER_BOUND('',#1237,.T.);
#853=FACE_OUTER_BOUND('',#1238,.T.);
#854=FACE_OUTER_BOUND('',#1239,.T.);
#855=FACE_OUTER_BOUND('',#1240,.T.);
#856=FACE_OUTER_BOUND('',#1241,.T.);
#857=FACE_OUTER_BOUND('',#1242,.T.);
#858=FACE_OUTER_BOUND('',#1243,.T.);
#859=FACE_OUTER_BOUND('',#1244,.T.);
#860=FACE_OUTER_BOUND('',#1245,.T.);
#861=FACE_OUTER_BOUND('',#1246,.T.);
#862=FACE_OUTER_BOUND('',#1247,.T.);
#863=FACE_OUTER_BOUND('',#1248,.T.);
#864=FACE_OUTER_BOUND('',#1249,.T.);
#865=FACE_OUTER_BOUND('',#1251,.T.);
#866=FACE_OUTER_BOUND('',#1252,.T.);
#867=FACE_OUTER_BOUND('',#1254,.T.);
#868=FACE_OUTER_BOUND('',#1255,.T.);
#869=FACE_OUTER_BOUND('',#1257,.T.);
#870=FACE_OUTER_BOUND('',#1258,.T.);
#871=FACE_OUTER_BOUND('',#1260,.T.);
#872=FACE_OUTER_BOUND('',#1261,.T.);
#873=FACE_OUTER_BOUND('',#1263,.T.);
#874=FACE_OUTER_BOUND('',#1264,.T.);
#875=FACE_OUTER_BOUND('',#1265,.T.);
#876=FACE_OUTER_BOUND('',#1266,.T.);
#877=FACE_OUTER_BOUND('',#1267,.T.);
#878=FACE_OUTER_BOUND('',#1268,.T.);
#879=FACE_OUTER_BOUND('',#1270,.T.);
#880=FACE_OUTER_BOUND('',#1271,.T.);
#881=FACE_OUTER_BOUND('',#1273,.T.);
#882=FACE_OUTER_BOUND('',#1274,.T.);
#883=FACE_OUTER_BOUND('',#1275,.T.);
#884=FACE_OUTER_BOUND('',#1276,.T.);
#885=FACE_OUTER_BOUND('',#1278,.T.);
#886=FACE_OUTER_BOUND('',#1280,.T.);
#887=FACE_OUTER_BOUND('',#1281,.T.);
#888=FACE_OUTER_BOUND('',#1283,.T.);
#889=FACE_OUTER_BOUND('',#1285,.T.);
#890=FACE_OUTER_BOUND('',#1286,.T.);
#891=FACE_OUTER_BOUND('',#1287,.T.);
#892=FACE_OUTER_BOUND('',#1290,.T.);
#893=FACE_OUTER_BOUND('',#1291,.T.);
#894=FACE_OUTER_BOUND('',#1292,.T.);
#895=FACE_OUTER_BOUND('',#1294,.T.);
#896=FACE_OUTER_BOUND('',#1295,.T.);
#897=FACE_OUTER_BOUND('',#1296,.T.);
#898=FACE_OUTER_BOUND('',#1298,.T.);
#899=FACE_OUTER_BOUND('',#1299,.T.);
#900=FACE_OUTER_BOUND('',#1300,.T.);
#901=FACE_OUTER_BOUND('',#1301,.T.);
#902=FACE_OUTER_BOUND('',#1303,.T.);
#903=FACE_OUTER_BOUND('',#1304,.T.);
#904=FACE_OUTER_BOUND('',#1305,.T.);
#905=FACE_OUTER_BOUND('',#1306,.T.);
#906=FACE_OUTER_BOUND('',#1308,.T.);
#907=FACE_OUTER_BOUND('',#1310,.T.);
#908=FACE_OUTER_BOUND('',#1311,.T.);
#909=FACE_OUTER_BOUND('',#1312,.T.);
#910=FACE_OUTER_BOUND('',#1314,.T.);
#911=FACE_OUTER_BOUND('',#1316,.T.);
#912=FACE_OUTER_BOUND('',#1317,.T.);
#913=FACE_OUTER_BOUND('',#1318,.T.);
#914=FACE_OUTER_BOUND('',#1319,.T.);
#915=FACE_OUTER_BOUND('',#1320,.T.);
#916=FACE_OUTER_BOUND('',#1322,.T.);
#917=FACE_OUTER_BOUND('',#1323,.T.);
#918=FACE_OUTER_BOUND('',#1324,.T.);
#919=FACE_OUTER_BOUND('',#1325,.T.);
#920=FACE_OUTER_BOUND('',#1326,.T.);
#921=FACE_OUTER_BOUND('',#1327,.T.);
#922=FACE_OUTER_BOUND('',#1328,.T.);
#923=FACE_OUTER_BOUND('',#1329,.T.);
#924=FACE_OUTER_BOUND('',#1330,.T.);
#925=FACE_OUTER_BOUND('',#1331,.T.);
#926=FACE_OUTER_BOUND('',#1332,.T.);
#927=FACE_OUTER_BOUND('',#1333,.T.);
#928=FACE_OUTER_BOUND('',#1334,.T.);
#929=FACE_OUTER_BOUND('',#1335,.T.);
#930=FACE_OUTER_BOUND('',#1336,.T.);
#931=FACE_OUTER_BOUND('',#1337,.T.);
#932=FACE_OUTER_BOUND('',#1338,.T.);
#933=FACE_OUTER_BOUND('',#1339,.T.);
#934=FACE_OUTER_BOUND('',#1340,.T.);
#935=FACE_OUTER_BOUND('',#1341,.T.);
#936=FACE_OUTER_BOUND('',#1342,.T.);
#937=FACE_OUTER_BOUND('',#1343,.T.);
#938=FACE_OUTER_BOUND('',#1344,.T.);
#939=FACE_OUTER_BOUND('',#1345,.T.);
#940=FACE_OUTER_BOUND('',#1346,.T.);
#941=FACE_OUTER_BOUND('',#1347,.T.);
#942=FACE_OUTER_BOUND('',#1349,.T.);
#943=FACE_OUTER_BOUND('',#1350,.T.);
#944=EDGE_LOOP('',(#3281,#3282,#3283,#3284));
#945=EDGE_LOOP('',(#3285,#3286,#3287,#3288));
#946=EDGE_LOOP('',(#3289,#3290,#3291,#3292));
#947=EDGE_LOOP('',(#3293,#3294,#3295,#3296));
#948=EDGE_LOOP('',(#3297,#3298,#3299,#3300));
#949=EDGE_LOOP('',(#3301,#3302,#3303,#3304));
#950=EDGE_LOOP('',(#3305,#3306,#3307,#3308));
#951=EDGE_LOOP('',(#3309,#3310,#3311,#3312));
#952=EDGE_LOOP('',(#3313,#3314,#3315,#3316));
#953=EDGE_LOOP('',(#3317));
#954=EDGE_LOOP('',(#3318));
#955=EDGE_LOOP('',(#3319));
#956=EDGE_LOOP('',(#3320));
#957=EDGE_LOOP('',(#3321,#3322,#3323,#3324));
#958=EDGE_LOOP('',(#3325));
#959=EDGE_LOOP('',(#3326));
#960=EDGE_LOOP('',(#3327));
#961=EDGE_LOOP('',(#3328));
#962=EDGE_LOOP('',(#3329,#3330,#3331,#3332));
#963=EDGE_LOOP('',(#3333,#3334,#3335,#3336));
#964=EDGE_LOOP('',(#3337,#3338,#3339,#3340));
#965=EDGE_LOOP('',(#3341,#3342,#3343,#3344));
#966=EDGE_LOOP('',(#3345,#3346,#3347,#3348));
#967=EDGE_LOOP('',(#3349,#3350,#3351,#3352));
#968=EDGE_LOOP('',(#3353,#3354,#3355,#3356));
#969=EDGE_LOOP('',(#3357,#3358,#3359,#3360));
#970=EDGE_LOOP('',(#3361,#3362,#3363,#3364));
#971=EDGE_LOOP('',(#3365,#3366,#3367,#3368));
#972=EDGE_LOOP('',(#3369,#3370,#3371,#3372));
#973=EDGE_LOOP('',(#3373,#3374,#3375,#3376));
#974=EDGE_LOOP('',(#3377,#3378));
#975=EDGE_LOOP('',(#3379));
#976=EDGE_LOOP('',(#3380,#3381,#3382,#3383));
#977=EDGE_LOOP('',(#3384,#3385));
#978=EDGE_LOOP('',(#3386));
#979=EDGE_LOOP('',(#3387,#3388,#3389,#3390));
#980=EDGE_LOOP('',(#3391,#3392));
#981=EDGE_LOOP('',(#3393));
#982=EDGE_LOOP('',(#3394,#3395,#3396,#3397));
#983=EDGE_LOOP('',(#3398,#3399));
#984=EDGE_LOOP('',(#3400));
#985=EDGE_LOOP('',(#3401,#3402,#3403,#3404));
#986=EDGE_LOOP('',(#3405,#3406,#3407,#3408,#3409,#3410,#3411,#3412,#3413));
#987=EDGE_LOOP('',(#3414));
#988=EDGE_LOOP('',(#3415,#3416,#3417,#3418,#3419,#3420,#3421,#3422,#3423,
#3424,#3425,#3426,#3427,#3428,#3429,#3430,#3431,#3432,#3433,#3434));
#989=EDGE_LOOP('',(#3435,#3436,#3437,#3438));
#990=EDGE_LOOP('',(#3439));
#991=EDGE_LOOP('',(#3440,#3441,#3442,#3443,#3444,#3445));
#992=EDGE_LOOP('',(#3446));
#993=EDGE_LOOP('',(#3447,#3448,#3449,#3450));
#994=EDGE_LOOP('',(#3451,#3452,#3453,#3454));
#995=EDGE_LOOP('',(#3455,#3456,#3457,#3458));
#996=EDGE_LOOP('',(#3459,#3460,#3461,#3462));
#997=EDGE_LOOP('',(#3463,#3464,#3465,#3466,#3467,#3468,#3469,#3470));
#998=EDGE_LOOP('',(#3471,#3472,#3473,#3474));
#999=EDGE_LOOP('',(#3475,#3476,#3477,#3478));
#1000=EDGE_LOOP('',(#3479,#3480,#3481,#3482));
#1001=EDGE_LOOP('',(#3483,#3484,#3485,#3486,#3487,#3488));
#1002=EDGE_LOOP('',(#3489,#3490,#3491,#3492,#3493,#3494,#3495,#3496));
#1003=EDGE_LOOP('',(#3497,#3498,#3499,#3500,#3501,#3502,#3503));
#1004=EDGE_LOOP('',(#3504,#3505,#3506,#3507));
#1005=EDGE_LOOP('',(#3508,#3509,#3510,#3511));
#1006=EDGE_LOOP('',(#3512,#3513,#3514,#3515));
#1007=EDGE_LOOP('',(#3516,#3517,#3518,#3519));
#1008=EDGE_LOOP('',(#3520,#3521,#3522,#3523));
#1009=EDGE_LOOP('',(#3524,#3525,#3526,#3527));
#1010=EDGE_LOOP('',(#3528,#3529,#3530,#3531));
#1011=EDGE_LOOP('',(#3532,#3533,#3534,#3535,#3536,#3537));
#1012=EDGE_LOOP('',(#3538));
#1013=EDGE_LOOP('',(#3539,#3540,#3541,#3542,#3543,#3544,#3545));
#1014=EDGE_LOOP('',(#3546,#3547,#3548,#3549,#3550,#3551));
#1015=EDGE_LOOP('',(#3552,#3553,#3554,#3555));
#1016=EDGE_LOOP('',(#3556,#3557,#3558,#3559,#3560));
#1017=EDGE_LOOP('',(#3561,#3562,#3563,#3564,#3565,#3566,#3567,#3568));
#1018=EDGE_LOOP('',(#3569));
#1019=EDGE_LOOP('',(#3570,#3571,#3572,#3573));
#1020=EDGE_LOOP('',(#3574,#3575,#3576,#3577));
#1021=EDGE_LOOP('',(#3578,#3579,#3580,#3581,#3582,#3583));
#1022=EDGE_LOOP('',(#3584));
#1023=EDGE_LOOP('',(#3585,#3586,#3587,#3588));
#1024=EDGE_LOOP('',(#3589,#3590,#3591,#3592));
#1025=EDGE_LOOP('',(#3593,#3594,#3595,#3596));
#1026=EDGE_LOOP('',(#3597,#3598,#3599,#3600));
#1027=EDGE_LOOP('',(#3601,#3602,#3603,#3604,#3605,#3606,#3607,#3608));
#1028=EDGE_LOOP('',(#3609));
#1029=EDGE_LOOP('',(#3610,#3611,#3612,#3613,#3614));
#1030=EDGE_LOOP('',(#3615,#3616,#3617,#3618));
#1031=EDGE_LOOP('',(#3619,#3620,#3621,#3622,#3623,#3624,#3625));
#1032=EDGE_LOOP('',(#3626,#3627,#3628,#3629,#3630,#3631));
#1033=EDGE_LOOP('',(#3632,#3633,#3634,#3635));
#1034=EDGE_LOOP('',(#3636,#3637,#3638,#3639));
#1035=EDGE_LOOP('',(#3640,#3641,#3642,#3643));
#1036=EDGE_LOOP('',(#3644,#3645,#3646,#3647));
#1037=EDGE_LOOP('',(#3648,#3649,#3650,#3651));
#1038=EDGE_LOOP('',(#3652));
#1039=EDGE_LOOP('',(#3653));
#1040=EDGE_LOOP('',(#3654,#3655,#3656,#3657));
#1041=EDGE_LOOP('',(#3658));
#1042=EDGE_LOOP('',(#3659));
#1043=EDGE_LOOP('',(#3660,#3661,#3662,#3663));
#1044=EDGE_LOOP('',(#3664));
#1045=EDGE_LOOP('',(#3665));
#1046=EDGE_LOOP('',(#3666));
#1047=EDGE_LOOP('',(#3667));
#1048=EDGE_LOOP('',(#3668));
#1049=EDGE_LOOP('',(#3669,#3670,#3671,#3672));
#1050=EDGE_LOOP('',(#3673,#3674,#3675,#3676));
#1051=EDGE_LOOP('',(#3677,#3678,#3679,#3680));
#1052=EDGE_LOOP('',(#3681,#3682,#3683,#3684));
#1053=EDGE_LOOP('',(#3685,#3686,#3687,#3688));
#1054=EDGE_LOOP('',(#3689,#3690,#3691,#3692));
#1055=EDGE_LOOP('',(#3693,#3694,#3695,#3696));
#1056=EDGE_LOOP('',(#3697));
#1057=EDGE_LOOP('',(#3698));
#1058=EDGE_LOOP('',(#3699,#3700,#3701,#3702));
#1059=EDGE_LOOP('',(#3703,#3704,#3705,#3706));
#1060=EDGE_LOOP('',(#3707,#3708,#3709,#3710));
#1061=EDGE_LOOP('',(#3711,#3712,#3713,#3714));
#1062=EDGE_LOOP('',(#3715,#3716,#3717,#3718));
#1063=EDGE_LOOP('',(#3719,#3720,#3721,#3722));
#1064=EDGE_LOOP('',(#3723,#3724,#3725,#3726,#3727,#3728));
#1065=EDGE_LOOP('',(#3729,#3730,#3731,#3732,#3733,#3734));
#1066=EDGE_LOOP('',(#3735));
#1067=EDGE_LOOP('',(#3736));
#1068=EDGE_LOOP('',(#3737,#3738,#3739,#3740));
#1069=EDGE_LOOP('',(#3741,#3742,#3743,#3744));
#1070=EDGE_LOOP('',(#3745,#3746,#3747,#3748));
#1071=EDGE_LOOP('',(#3749));
#1072=EDGE_LOOP('',(#3750));
#1073=EDGE_LOOP('',(#3751,#3752,#3753,#3754));
#1074=EDGE_LOOP('',(#3755,#3756,#3757,#3758));
#1075=EDGE_LOOP('',(#3759,#3760,#3761,#3762));
#1076=EDGE_LOOP('',(#3763));
#1077=EDGE_LOOP('',(#3764,#3765,#3766,#3767));
#1078=EDGE_LOOP('',(#3768));
#1079=EDGE_LOOP('',(#3769,#3770,#3771,#3772));
#1080=EDGE_LOOP('',(#3773));
#1081=EDGE_LOOP('',(#3774,#3775,#3776,#3777));
#1082=EDGE_LOOP('',(#3778));
#1083=EDGE_LOOP('',(#3779,#3780,#3781,#3782));
#1084=EDGE_LOOP('',(#3783));
#1085=EDGE_LOOP('',(#3784,#3785,#3786,#3787));
#1086=EDGE_LOOP('',(#3788));
#1087=EDGE_LOOP('',(#3789,#3790,#3791,#3792));
#1088=EDGE_LOOP('',(#3793));
#1089=EDGE_LOOP('',(#3794,#3795,#3796,#3797));
#1090=EDGE_LOOP('',(#3798));
#1091=EDGE_LOOP('',(#3799,#3800,#3801,#3802));
#1092=EDGE_LOOP('',(#3803));
#1093=EDGE_LOOP('',(#3804,#3805,#3806,#3807));
#1094=EDGE_LOOP('',(#3808,#3809,#3810,#3811));
#1095=EDGE_LOOP('',(#3812));
#1096=EDGE_LOOP('',(#3813,#3814,#3815,#3816));
#1097=EDGE_LOOP('',(#3817,#3818,#3819,#3820));
#1098=EDGE_LOOP('',(#3821,#3822,#3823,#3824));
#1099=EDGE_LOOP('',(#3825,#3826,#3827,#3828));
#1100=EDGE_LOOP('',(#3829,#3830,#3831,#3832));
#1101=EDGE_LOOP('',(#3833,#3834,#3835,#3836));
#1102=EDGE_LOOP('',(#3837));
#1103=EDGE_LOOP('',(#3838));
#1104=EDGE_LOOP('',(#3839));
#1105=EDGE_LOOP('',(#3840));
#1106=EDGE_LOOP('',(#3841));
#1107=EDGE_LOOP('',(#3842));
#1108=EDGE_LOOP('',(#3843));
#1109=EDGE_LOOP('',(#3844));
#1110=EDGE_LOOP('',(#3845));
#1111=EDGE_LOOP('',(#3846));
#1112=EDGE_LOOP('',(#3847));
#1113=EDGE_LOOP('',(#3848));
#1114=EDGE_LOOP('',(#3849,#3850,#3851,#3852));
#1115=EDGE_LOOP('',(#3853,#3854,#3855,#3856));
#1116=EDGE_LOOP('',(#3857));
#1117=EDGE_LOOP('',(#3858));
#1118=EDGE_LOOP('',(#3859));
#1119=EDGE_LOOP('',(#3860));
#1120=EDGE_LOOP('',(#3861,#3862,#3863,#3864));
#1121=EDGE_LOOP('',(#3865,#3866,#3867,#3868));
#1122=EDGE_LOOP('',(#3869));
#1123=EDGE_LOOP('',(#3870));
#1124=EDGE_LOOP('',(#3871));
#1125=EDGE_LOOP('',(#3872));
#1126=EDGE_LOOP('',(#3873,#3874,#3875,#3876));
#1127=EDGE_LOOP('',(#3877));
#1128=EDGE_LOOP('',(#3878));
#1129=EDGE_LOOP('',(#3879,#3880,#3881,#3882));
#1130=EDGE_LOOP('',(#3883));
#1131=EDGE_LOOP('',(#3884));
#1132=EDGE_LOOP('',(#3885,#3886,#3887,#3888));
#1133=EDGE_LOOP('',(#3889));
#1134=EDGE_LOOP('',(#3890));
#1135=EDGE_LOOP('',(#3891,#3892,#3893,#3894));
#1136=EDGE_LOOP('',(#3895));
#1137=EDGE_LOOP('',(#3896));
#1138=EDGE_LOOP('',(#3897,#3898,#3899,#3900));
#1139=EDGE_LOOP('',(#3901,#3902,#3903,#3904));
#1140=EDGE_LOOP('',(#3905,#3906,#3907,#3908));
#1141=EDGE_LOOP('',(#3909,#3910,#3911,#3912));
#1142=EDGE_LOOP('',(#3913,#3914,#3915,#3916));
#1143=EDGE_LOOP('',(#3917));
#1144=EDGE_LOOP('',(#3918));
#1145=EDGE_LOOP('',(#3919,#3920,#3921,#3922));
#1146=EDGE_LOOP('',(#3923,#3924,#3925,#3926));
#1147=EDGE_LOOP('',(#3927));
#1148=EDGE_LOOP('',(#3928));
#1149=EDGE_LOOP('',(#3929));
#1150=EDGE_LOOP('',(#3930));
#1151=EDGE_LOOP('',(#3931));
#1152=EDGE_LOOP('',(#3932));
#1153=EDGE_LOOP('',(#3933));
#1154=EDGE_LOOP('',(#3934));
#1155=EDGE_LOOP('',(#3935));
#1156=EDGE_LOOP('',(#3936));
#1157=EDGE_LOOP('',(#3937));
#1158=EDGE_LOOP('',(#3938));
#1159=EDGE_LOOP('',(#3939,#3940,#3941,#3942));
#1160=EDGE_LOOP('',(#3943));
#1161=EDGE_LOOP('',(#3944));
#1162=EDGE_LOOP('',(#3945,#3946,#3947,#3948));
#1163=EDGE_LOOP('',(#3949));
#1164=EDGE_LOOP('',(#3950));
#1165=EDGE_LOOP('',(#3951,#3952,#3953,#3954));
#1166=EDGE_LOOP('',(#3955));
#1167=EDGE_LOOP('',(#3956));
#1168=EDGE_LOOP('',(#3957,#3958,#3959,#3960));
#1169=EDGE_LOOP('',(#3961));
#1170=EDGE_LOOP('',(#3962));
#1171=EDGE_LOOP('',(#3963,#3964,#3965,#3966));
#1172=EDGE_LOOP('',(#3967,#3968,#3969,#3970));
#1173=EDGE_LOOP('',(#3971,#3972,#3973,#3974));
#1174=EDGE_LOOP('',(#3975,#3976,#3977,#3978));
#1175=EDGE_LOOP('',(#3979,#3980,#3981,#3982));
#1176=EDGE_LOOP('',(#3983,#3984,#3985,#3986));
#1177=EDGE_LOOP('',(#3987,#3988,#3989,#3990));
#1178=EDGE_LOOP('',(#3991,#3992,#3993,#3994));
#1179=EDGE_LOOP('',(#3995));
#1180=EDGE_LOOP('',(#3996));
#1181=EDGE_LOOP('',(#3997,#3998,#3999,#4000));
#1182=EDGE_LOOP('',(#4001,#4002,#4003,#4004));
#1183=EDGE_LOOP('',(#4005,#4006,#4007,#4008));
#1184=EDGE_LOOP('',(#4009));
#1185=EDGE_LOOP('',(#4010));
#1186=EDGE_LOOP('',(#4011));
#1187=EDGE_LOOP('',(#4012));
#1188=EDGE_LOOP('',(#4013));
#1189=EDGE_LOOP('',(#4014,#4015,#4016,#4017));
#1190=EDGE_LOOP('',(#4018));
#1191=EDGE_LOOP('',(#4019));
#1192=EDGE_LOOP('',(#4020));
#1193=EDGE_LOOP('',(#4021));
#1194=EDGE_LOOP('',(#4022));
#1195=EDGE_LOOP('',(#4023,#4024,#4025,#4026));
#1196=EDGE_LOOP('',(#4027));
#1197=EDGE_LOOP('',(#4028,#4029,#4030,#4031));
#1198=EDGE_LOOP('',(#4032));
#1199=EDGE_LOOP('',(#4033));
#1200=EDGE_LOOP('',(#4034));
#1201=EDGE_LOOP('',(#4035,#4036,#4037,#4038));
#1202=EDGE_LOOP('',(#4039));
#1203=EDGE_LOOP('',(#4040));
#1204=EDGE_LOOP('',(#4041,#4042,#4043,#4044,#4045,#4046));
#1205=EDGE_LOOP('',(#4047,#4048,#4049,#4050,#4051));
#1206=EDGE_LOOP('',(#4052,#4053,#4054,#4055));
#1207=EDGE_LOOP('',(#4056,#4057,#4058,#4059));
#1208=EDGE_LOOP('',(#4060));
#1209=EDGE_LOOP('',(#4061));
#1210=EDGE_LOOP('',(#4062,#4063,#4064,#4065,#4066));
#1211=EDGE_LOOP('',(#4067));
#1212=EDGE_LOOP('',(#4068));
#1213=EDGE_LOOP('',(#4069,#4070,#4071,#4072));
#1214=EDGE_LOOP('',(#4073,#4074,#4075,#4076,#4077,#4078));
#1215=EDGE_LOOP('',(#4079,#4080,#4081,#4082,#4083));
#1216=EDGE_LOOP('',(#4084));
#1217=EDGE_LOOP('',(#4085));
#1218=EDGE_LOOP('',(#4086,#4087,#4088,#4089));
#1219=EDGE_LOOP('',(#4090,#4091,#4092,#4093));
#1220=EDGE_LOOP('',(#4094,#4095,#4096,#4097));
#1221=EDGE_LOOP('',(#4098));
#1222=EDGE_LOOP('',(#4099));
#1223=EDGE_LOOP('',(#4100,#4101,#4102,#4103,#4104));
#1224=EDGE_LOOP('',(#4105,#4106));
#1225=EDGE_LOOP('',(#4107,#4108));
#1226=EDGE_LOOP('',(#4109,#4110));
#1227=EDGE_LOOP('',(#4111,#4112));
#1228=EDGE_LOOP('',(#4113,#4114));
#1229=EDGE_LOOP('',(#4115,#4116));
#1230=EDGE_LOOP('',(#4117,#4118));
#1231=EDGE_LOOP('',(#4119,#4120));
#1232=EDGE_LOOP('',(#4121,#4122,#4123,#4124));
#1233=EDGE_LOOP('',(#4125,#4126,#4127,#4128,#4129,#4130,#4131,#4132,#4133,
#4134,#4135,#4136,#4137,#4138,#4139,#4140,#4141,#4142,#4143,#4144));
#1234=EDGE_LOOP('',(#4145,#4146,#4147,#4148));
#1235=EDGE_LOOP('',(#4149,#4150,#4151,#4152));
#1236=EDGE_LOOP('',(#4153,#4154,#4155,#4156));
#1237=EDGE_LOOP('',(#4157,#4158,#4159,#4160));
#1238=EDGE_LOOP('',(#4161,#4162,#4163,#4164));
#1239=EDGE_LOOP('',(#4165,#4166,#4167,#4168,#4169,#4170));
#1240=EDGE_LOOP('',(#4171,#4172,#4173,#4174));
#1241=EDGE_LOOP('',(#4175,#4176,#4177,#4178));
#1242=EDGE_LOOP('',(#4179,#4180,#4181,#4182));
#1243=EDGE_LOOP('',(#4183,#4184,#4185,#4186));
#1244=EDGE_LOOP('',(#4187,#4188,#4189,#4190));
#1245=EDGE_LOOP('',(#4191,#4192,#4193,#4194));
#1246=EDGE_LOOP('',(#4195,#4196,#4197,#4198,#4199,#4200,#4201,#4202,#4203,
#4204,#4205,#4206,#4207,#4208,#4209,#4210,#4211,#4212,#4213,#4214));
#1247=EDGE_LOOP('',(#4215,#4216,#4217,#4218));
#1248=EDGE_LOOP('',(#4219,#4220,#4221,#4222));
#1249=EDGE_LOOP('',(#4223));
#1250=EDGE_LOOP('',(#4224));
#1251=EDGE_LOOP('',(#4225,#4226,#4227,#4228));
#1252=EDGE_LOOP('',(#4229));
#1253=EDGE_LOOP('',(#4230));
#1254=EDGE_LOOP('',(#4231,#4232,#4233,#4234));
#1255=EDGE_LOOP('',(#4235));
#1256=EDGE_LOOP('',(#4236));
#1257=EDGE_LOOP('',(#4237,#4238,#4239,#4240));
#1258=EDGE_LOOP('',(#4241));
#1259=EDGE_LOOP('',(#4242));
#1260=EDGE_LOOP('',(#4243,#4244,#4245,#4246));
#1261=EDGE_LOOP('',(#4247));
#1262=EDGE_LOOP('',(#4248));
#1263=EDGE_LOOP('',(#4249,#4250,#4251,#4252));
#1264=EDGE_LOOP('',(#4253,#4254,#4255,#4256));
#1265=EDGE_LOOP('',(#4257));
#1266=EDGE_LOOP('',(#4258,#4259,#4260,#4261));
#1267=EDGE_LOOP('',(#4262));
#1268=EDGE_LOOP('',(#4263));
#1269=EDGE_LOOP('',(#4264));
#1270=EDGE_LOOP('',(#4265,#4266,#4267,#4268));
#1271=EDGE_LOOP('',(#4269));
#1272=EDGE_LOOP('',(#4270));
#1273=EDGE_LOOP('',(#4271,#4272,#4273,#4274));
#1274=EDGE_LOOP('',(#4275,#4276,#4277,#4278));
#1275=EDGE_LOOP('',(#4279,#4280,#4281,#4282));
#1276=EDGE_LOOP('',(#4283));
#1277=EDGE_LOOP('',(#4284));
#1278=EDGE_LOOP('',(#4285));
#1279=EDGE_LOOP('',(#4286));
#1280=EDGE_LOOP('',(#4287,#4288,#4289,#4290));
#1281=EDGE_LOOP('',(#4291));
#1282=EDGE_LOOP('',(#4292));
#1283=EDGE_LOOP('',(#4293));
#1284=EDGE_LOOP('',(#4294));
#1285=EDGE_LOOP('',(#4295,#4296,#4297,#4298));
#1286=EDGE_LOOP('',(#4299,#4300,#4301,#4302));
#1287=EDGE_LOOP('',(#4303,#4304,#4305,#4306,#4307));
#1288=EDGE_LOOP('',(#4308));
#1289=EDGE_LOOP('',(#4309));
#1290=EDGE_LOOP('',(#4310,#4311,#4312,#4313));
#1291=EDGE_LOOP('',(#4314,#4315,#4316,#4317));
#1292=EDGE_LOOP('',(#4318,#4319,#4320,#4321));
#1293=EDGE_LOOP('',(#4322));
#1294=EDGE_LOOP('',(#4323,#4324,#4325,#4326));
#1295=EDGE_LOOP('',(#4327,#4328,#4329,#4330,#4331,#4332,#4333,#4334));
#1296=EDGE_LOOP('',(#4335));
#1297=EDGE_LOOP('',(#4336));
#1298=EDGE_LOOP('',(#4337,#4338,#4339,#4340));
#1299=EDGE_LOOP('',(#4341));
#1300=EDGE_LOOP('',(#4342,#4343,#4344,#4345));
#1301=EDGE_LOOP('',(#4346));
#1302=EDGE_LOOP('',(#4347));
#1303=EDGE_LOOP('',(#4348));
#1304=EDGE_LOOP('',(#4349,#4350,#4351,#4352));
#1305=EDGE_LOOP('',(#4353,#4354,#4355,#4356));
#1306=EDGE_LOOP('',(#4357));
#1307=EDGE_LOOP('',(#4358));
#1308=EDGE_LOOP('',(#4359));
#1309=EDGE_LOOP('',(#4360));
#1310=EDGE_LOOP('',(#4361,#4362,#4363,#4364));
#1311=EDGE_LOOP('',(#4365,#4366,#4367,#4368));
#1312=EDGE_LOOP('',(#4369));
#1313=EDGE_LOOP('',(#4370));
#1314=EDGE_LOOP('',(#4371));
#1315=EDGE_LOOP('',(#4372));
#1316=EDGE_LOOP('',(#4373));
#1317=EDGE_LOOP('',(#4374,#4375,#4376,#4377));
#1318=EDGE_LOOP('',(#4378,#4379,#4380,#4381));
#1319=EDGE_LOOP('',(#4382,#4383,#4384,#4385));
#1320=EDGE_LOOP('',(#4386));
#1321=EDGE_LOOP('',(#4387));
#1322=EDGE_LOOP('',(#4388,#4389,#4390,#4391));
#1323=EDGE_LOOP('',(#4392,#4393,#4394,#4395));
#1324=EDGE_LOOP('',(#4396,#4397,#4398,#4399));
#1325=EDGE_LOOP('',(#4400));
#1326=EDGE_LOOP('',(#4401,#4402,#4403,#4404));
#1327=EDGE_LOOP('',(#4405,#4406,#4407,#4408));
#1328=EDGE_LOOP('',(#4409,#4410,#4411,#4412));
#1329=EDGE_LOOP('',(#4413,#4414,#4415,#4416));
#1330=EDGE_LOOP('',(#4417,#4418,#4419,#4420));
#1331=EDGE_LOOP('',(#4421,#4422,#4423,#4424));
#1332=EDGE_LOOP('',(#4425,#4426,#4427,#4428,#4429,#4430));
#1333=EDGE_LOOP('',(#4431,#4432,#4433,#4434,#4435,#4436));
#1334=EDGE_LOOP('',(#4437,#4438,#4439,#4440));
#1335=EDGE_LOOP('',(#4441,#4442,#4443,#4444));
#1336=EDGE_LOOP('',(#4445,#4446,#4447,#4448));
#1337=EDGE_LOOP('',(#4449,#4450,#4451,#4452));
#1338=EDGE_LOOP('',(#4453,#4454,#4455,#4456));
#1339=EDGE_LOOP('',(#4457,#4458,#4459,#4460));
#1340=EDGE_LOOP('',(#4461,#4462,#4463,#4464,#4465,#4466));
#1341=EDGE_LOOP('',(#4467,#4468,#4469,#4470,#4471,#4472));
#1342=EDGE_LOOP('',(#4473));
#1343=EDGE_LOOP('',(#4474));
#1344=EDGE_LOOP('',(#4475,#4476,#4477,#4478));
#1345=EDGE_LOOP('',(#4479,#4480,#4481,#4482));
#1346=EDGE_LOOP('',(#4483,#4484,#4485,#4486));
#1347=EDGE_LOOP('',(#4487));
#1348=EDGE_LOOP('',(#4488));
#1349=EDGE_LOOP('',(#4489,#4490,#4491,#4492));
#1350=EDGE_LOOP('',(#4493,#4494,#4495,#4496));
#1351=LINE('',#7493,#1673);
#1352=LINE('',#7499,#1674);
#1353=LINE('',#7505,#1675);
#1354=LINE('',#7511,#1676);
#1355=LINE('',#7516,#1677);
#1356=LINE('',#7518,#1678);
#1357=LINE('',#7520,#1679);
#1358=LINE('',#7521,#1680);
#1359=LINE('',#7524,#1681);
#1360=LINE('',#7526,#1682);
#1361=LINE('',#7527,#1683);
#1362=LINE('',#7530,#1684);
#1363=LINE('',#7532,#1685);
#1364=LINE('',#7533,#1686);
#1365=LINE('',#7535,#1687);
#1366=LINE('',#7536,#1688);
#1367=LINE('',#7543,#1689);
#1368=LINE('',#7545,#1690);
#1369=LINE('',#7547,#1691);
#1370=LINE('',#7548,#1692);
#1371=LINE('',#7551,#1693);
#1372=LINE('',#7553,#1694);
#1373=LINE('',#7554,#1695);
#1374=LINE('',#7557,#1696);
#1375=LINE('',#7559,#1697);
#1376=LINE('',#7560,#1698);
#1377=LINE('',#7562,#1699);
#1378=LINE('',#7563,#1700);
#1379=LINE('',#7570,#1701);
#1380=LINE('',#7572,#1702);
#1381=LINE('',#7574,#1703);
#1382=LINE('',#7575,#1704);
#1383=LINE('',#7578,#1705);
#1384=LINE('',#7580,#1706);
#1385=LINE('',#7581,#1707);
#1386=LINE('',#7584,#1708);
#1387=LINE('',#7586,#1709);
#1388=LINE('',#7587,#1710);
#1389=LINE('',#7589,#1711);
#1390=LINE('',#7590,#1712);
#1391=LINE('',#7603,#1713);
#1392=LINE('',#7606,#1714);
#1393=LINE('',#7616,#1715);
#1394=LINE('',#7619,#1716);
#1395=LINE('',#7629,#1717);
#1396=LINE('',#7632,#1718);
#1397=LINE('',#7642,#1719);
#1398=LINE('',#7645,#1720);
#1399=LINE('',#7657,#1721);
#1400=LINE('',#7663,#1722);
#1401=LINE('',#7669,#1723);
#1402=LINE('',#7671,#1724);
#1403=LINE('',#7673,#1725);
#1404=LINE('',#7675,#1726);
#1405=LINE('',#7677,#1727);
#1406=LINE('',#7678,#1728);
#1407=LINE('',#7681,#1729);
#1408=LINE('',#7683,#1730);
#1409=LINE('',#7684,#1731);
#1410=LINE('',#7688,#1732);
#1411=LINE('',#7689,#1733);
#1412=LINE('',#7690,#1734);
#1413=LINE('',#7692,#1735);
#1414=LINE('',#7695,#1736);
#1415=LINE('',#7697,#1737);
#1416=LINE('',#7698,#1738);
#1417=LINE('',#7701,#1739);
#1418=LINE('',#7703,#1740);
#1419=LINE('',#7705,#1741);
#1420=LINE('',#7708,#1742);
#1421=LINE('',#7711,#1743);
#1422=LINE('',#7712,#1744);
#1423=LINE('',#7715,#1745);
#1424=LINE('',#7717,#1746);
#1425=LINE('',#7718,#1747);
#1426=LINE('',#7721,#1748);
#1427=LINE('',#7722,#1749);
#1428=LINE('',#7724,#1750);
#1429=LINE('',#7729,#1751);
#1430=LINE('',#7733,#1752);
#1431=LINE('',#7737,#1753);
#1432=LINE('',#7741,#1754);
#1433=LINE('',#7745,#1755);
#1434=LINE('',#7751,#1756);
#1435=LINE('',#7756,#1757);
#1436=LINE('',#7758,#1758);
#1437=LINE('',#7760,#1759);
#1438=LINE('',#7761,#1760);
#1439=LINE('',#7765,#1761);
#1440=LINE('',#7767,#1762);
#1441=LINE('',#7769,#1763);
#1442=LINE('',#7770,#1764);
#1443=LINE('',#7773,#1765);
#1444=LINE('',#7775,#1766);
#1445=LINE('',#7776,#1767);
#1446=LINE('',#7778,#1768);
#1447=LINE('',#7779,#1769);
#1448=LINE('',#7782,#1770);
#1449=LINE('',#7783,#1771);
#1450=LINE('',#7786,#1772);
#1451=LINE('',#7787,#1773);
#1452=LINE('',#7789,#1774);
#1453=LINE('',#7790,#1775);
#1454=LINE('',#7793,#1776);
#1455=LINE('',#7795,#1777);
#1456=LINE('',#7796,#1778);
#1457=LINE('',#7799,#1779);
#1458=LINE('',#7800,#1780);
#1459=LINE('',#7802,#1781);
#1460=LINE('',#7803,#1782);
#1461=LINE('',#7810,#1783);
#1462=LINE('',#7815,#1784);
#1463=LINE('',#7817,#1785);
#1464=LINE('',#7819,#1786);
#1465=LINE('',#7821,#1787);
#1466=LINE('',#7823,#1788);
#1467=LINE('',#7824,#1789);
#1468=LINE('',#7827,#1790);
#1469=LINE('',#7829,#1791);
#1470=LINE('',#7830,#1792);
#1471=LINE('',#7833,#1793);
#1472=LINE('',#7835,#1794);
#1473=LINE('',#7836,#1795);
#1474=LINE('',#7839,#1796);
#1475=LINE('',#7840,#1797);
#1476=LINE('',#7842,#1798);
#1477=LINE('',#7845,#1799);
#1478=LINE('',#7847,#1800);
#1479=LINE('',#7849,#1801);
#1480=LINE('',#7850,#1802);
#1481=LINE('',#7852,#1803);
#1482=LINE('',#7854,#1804);
#1483=LINE('',#7855,#1805);
#1484=LINE('',#7857,#1806);
#1485=LINE('',#7860,#1807);
#1486=LINE('',#7861,#1808);
#1487=LINE('',#7863,#1809);
#1488=LINE('',#7868,#1810);
#1489=LINE('',#7872,#1811);
#1490=LINE('',#7876,#1812);
#1491=LINE('',#7880,#1813);
#1492=LINE('',#7889,#1814);
#1493=LINE('',#7892,#1815);
#1494=LINE('',#7898,#1816);
#1495=LINE('',#7900,#1817);
#1496=LINE('',#7902,#1818);
#1497=LINE('',#7903,#1819);
#1498=LINE('',#7906,#1820);
#1499=LINE('',#7908,#1821);
#1500=LINE('',#7909,#1822);
#1501=LINE('',#7912,#1823);
#1502=LINE('',#7914,#1824);
#1503=LINE('',#7915,#1825);
#1504=LINE('',#7917,#1826);
#1505=LINE('',#7918,#1827);
#1506=LINE('',#9274,#1828);
#1507=LINE('',#9276,#1829);
#1508=LINE('',#9278,#1830);
#1509=LINE('',#9279,#1831);
#1510=LINE('',#9282,#1832);
#1511=LINE('',#9284,#1833);
#1512=LINE('',#9285,#1834);
#1513=LINE('',#9288,#1835);
#1514=LINE('',#9290,#1836);
#1515=LINE('',#9291,#1837);
#1516=LINE('',#9294,#1838);
#1517=LINE('',#9296,#1839);
#1518=LINE('',#9297,#1840);
#1519=LINE('',#9300,#1841);
#1520=LINE('',#9302,#1842);
#1521=LINE('',#9303,#1843);
#1522=LINE('',#9305,#1844);
#1523=LINE('',#9306,#1845);
#1524=LINE('',#9318,#1846);
#1525=LINE('',#9322,#1847);
#1526=LINE('',#9326,#1848);
#1527=LINE('',#9333,#1849);
#1528=LINE('',#9335,#1850);
#1529=LINE('',#9352,#1851);
#1530=LINE('',#9359,#1852);
#1531=LINE('',#9366,#1853);
#1532=LINE('',#9373,#1854);
#1533=LINE('',#9380,#1855);
#1534=LINE('',#9387,#1856);
#1535=LINE('',#9394,#1857);
#1536=LINE('',#9401,#1858);
#1537=LINE('',#9408,#1859);
#1538=LINE('',#9414,#1860);
#1539=LINE('',#9418,#1861);
#1540=LINE('',#9422,#1862);
#1541=LINE('',#9425,#1863);
#1542=LINE('',#9428,#1864);
#1543=LINE('',#9429,#1865);
#1544=LINE('',#9432,#1866);
#1545=LINE('',#9433,#1867);
#1546=LINE('',#9440,#1868);
#1547=LINE('',#9446,#1869);
#1548=LINE('',#9455,#1870);
#1549=LINE('',#9461,#1871);
#1550=LINE('',#9470,#1872);
#1551=LINE('',#9476,#1873);
#1552=LINE('',#9485,#1874);
#1553=LINE('',#9494,#1875);
#1554=LINE('',#9503,#1876);
#1555=LINE('',#9512,#1877);
#1556=LINE('',#9519,#1878);
#1557=LINE('',#9523,#1879);
#1558=LINE('',#9527,#1880);
#1559=LINE('',#9531,#1881);
#1560=LINE('',#9537,#1882);
#1561=LINE('',#9544,#1883);
#1562=LINE('',#9550,#1884);
#1563=LINE('',#9559,#1885);
#1564=LINE('',#9568,#1886);
#1565=LINE('',#9577,#1887);
#1566=LINE('',#9586,#1888);
#1567=LINE('',#9594,#1889);
#1568=LINE('',#9598,#1890);
#1569=LINE('',#9602,#1891);
#1570=LINE('',#9606,#1892);
#1571=LINE('',#9610,#1893);
#1572=LINE('',#9612,#1894);
#1573=LINE('',#9614,#1895);
#1574=LINE('',#9615,#1896);
#1575=LINE('',#9619,#1897);
#1576=LINE('',#9621,#1898);
#1577=LINE('',#9623,#1899);
#1578=LINE('',#9624,#1900);
#1579=LINE('',#9626,#1901);
#1580=LINE('',#9627,#1902);
#1581=LINE('',#9632,#1903);
#1582=LINE('',#9640,#1904);
#1583=LINE('',#9651,#1905);
#1584=LINE('',#9658,#1906);
#1585=LINE('',#9667,#1907);
#1586=LINE('',#9685,#1908);
#1587=LINE('',#9691,#1909);
#1588=LINE('',#9695,#1910);
#1589=LINE('',#9701,#1911);
#1590=LINE('',#9706,#1912);
#1591=LINE('',#9721,#1913);
#1592=LINE('',#9730,#1914);
#1593=LINE('',#9734,#1915);
#1594=LINE('',#9738,#1916);
#1595=LINE('',#9741,#1917);
#1596=LINE('',#9894,#1918);
#1597=LINE('',#10190,#1919);
#1598=LINE('',#10232,#1920);
#1599=LINE('',#10237,#1921);
#1600=LINE('',#10246,#1922);
#1601=LINE('',#10251,#1923);
#1602=LINE('',#10263,#1924);
#1603=LINE('',#10270,#1925);
#1604=LINE('',#10280,#1926);
#1605=LINE('',#10290,#1927);
#1606=LINE('',#10293,#1928);
#1607=LINE('',#10298,#1929);
#1608=LINE('',#10305,#1930);
#1609=LINE('',#10314,#1931);
#1610=LINE('',#10319,#1932);
#1611=LINE('',#10323,#1933);
#1612=LINE('',#10327,#1934);
#1613=LINE('',#10332,#1935);
#1614=LINE('',#10337,#1936);
#1615=LINE('',#10338,#1937);
#1616=LINE('',#10341,#1938);
#1617=LINE('',#10342,#1939);
#1618=LINE('',#10348,#1940);
#1619=LINE('',#10352,#1941);
#1620=LINE('',#10359,#1942);
#1621=LINE('',#10366,#1943);
#1622=LINE('',#10375,#1944);
#1623=LINE('',#10381,#1945);
#1624=LINE('',#10390,#1946);
#1625=LINE('',#10396,#1947);
#1626=LINE('',#10407,#1948);
#1627=LINE('',#10411,#1949);
#1628=LINE('',#10415,#1950);
#1629=LINE('',#10422,#1951);
#1630=LINE('',#10426,#1952);
#1631=LINE('',#10430,#1953);
#1632=LINE('',#10435,#1954);
#1633=LINE('',#10437,#1955);
#1634=LINE('',#10439,#1956);
#1635=LINE('',#10440,#1957);
#1636=LINE('',#10443,#1958);
#1637=LINE('',#10445,#1959);
#1638=LINE('',#10446,#1960);
#1639=LINE('',#10449,#1961);
#1640=LINE('',#10451,#1962);
#1641=LINE('',#10452,#1963);
#1642=LINE('',#10455,#1964);
#1643=LINE('',#10457,#1965);
#1644=LINE('',#10458,#1966);
#1645=LINE('',#10461,#1967);
#1646=LINE('',#10463,#1968);
#1647=LINE('',#10464,#1969);
#1648=LINE('',#10466,#1970);
#1649=LINE('',#10467,#1971);
#1650=LINE('',#10474,#1972);
#1651=LINE('',#10476,#1973);
#1652=LINE('',#10478,#1974);
#1653=LINE('',#10479,#1975);
#1654=LINE('',#10482,#1976);
#1655=LINE('',#10484,#1977);
#1656=LINE('',#10485,#1978);
#1657=LINE('',#10488,#1979);
#1658=LINE('',#10490,#1980);
#1659=LINE('',#10491,#1981);
#1660=LINE('',#10494,#1982);
#1661=LINE('',#10496,#1983);
#1662=LINE('',#10497,#1984);
#1663=LINE('',#10500,#1985);
#1664=LINE('',#10502,#1986);
#1665=LINE('',#10503,#1987);
#1666=LINE('',#10505,#1988);
#1667=LINE('',#10506,#1989);
#1668=LINE('',#10518,#1990);
#1669=LINE('',#10522,#1991);
#1670=LINE('',#10526,#1992);
#1671=LINE('',#10533,#1993);
#1672=LINE('',#10535,#1994);
#1673=VECTOR('',#5880,0.21);
#1674=VECTOR('',#5887,0.21);
#1675=VECTOR('',#5894,0.21);
#1676=VECTOR('',#5901,0.21);
#1677=VECTOR('',#5906,1.);
#1678=VECTOR('',#5907,1.);
#1679=VECTOR('',#5908,1.);
#1680=VECTOR('',#5909,1.);
#1681=VECTOR('',#5912,1.);
#1682=VECTOR('',#5913,1.);
#1683=VECTOR('',#5914,1.);
#1684=VECTOR('',#5917,1.);
#1685=VECTOR('',#5918,1.);
#1686=VECTOR('',#5919,1.);
#1687=VECTOR('',#5922,1.);
#1688=VECTOR('',#5923,1.);
#1689=VECTOR('',#5932,1.);
#1690=VECTOR('',#5933,1.);
#1691=VECTOR('',#5934,1.);
#1692=VECTOR('',#5935,1.);
#1693=VECTOR('',#5938,1.);
#1694=VECTOR('',#5939,1.);
#1695=VECTOR('',#5940,1.);
#1696=VECTOR('',#5943,1.);
#1697=VECTOR('',#5944,1.);
#1698=VECTOR('',#5945,1.);
#1699=VECTOR('',#5948,1.);
#1700=VECTOR('',#5949,1.);
#1701=VECTOR('',#5958,1.);
#1702=VECTOR('',#5959,1.);
#1703=VECTOR('',#5960,1.);
#1704=VECTOR('',#5961,1.);
#1705=VECTOR('',#5964,1.);
#1706=VECTOR('',#5965,1.);
#1707=VECTOR('',#5966,1.);
#1708=VECTOR('',#5969,1.);
#1709=VECTOR('',#5970,1.);
#1710=VECTOR('',#5971,1.);
#1711=VECTOR('',#5974,1.);
#1712=VECTOR('',#5975,1.);
#1713=VECTOR('',#5992,1.);
#1714=VECTOR('',#5995,1.);
#1715=VECTOR('',#6006,1.);
#1716=VECTOR('',#6009,1.);
#1717=VECTOR('',#6020,1.);
#1718=VECTOR('',#6023,1.);
#1719=VECTOR('',#6034,1.);
#1720=VECTOR('',#6037,1.);
#1721=VECTOR('',#6054,1.8);
#1722=VECTOR('',#6061,0.3);
#1723=VECTOR('',#6068,1.);
#1724=VECTOR('',#6069,1.);
#1725=VECTOR('',#6070,1.);
#1726=VECTOR('',#6071,1.);
#1727=VECTOR('',#6072,1.);
#1728=VECTOR('',#6073,1.);
#1729=VECTOR('',#6076,1.);
#1730=VECTOR('',#6077,1.);
#1731=VECTOR('',#6078,1.);
#1732=VECTOR('',#6081,1.);
#1733=VECTOR('',#6082,1.);
#1734=VECTOR('',#6083,1.);
#1735=VECTOR('',#6086,1.);
#1736=VECTOR('',#6089,1.);
#1737=VECTOR('',#6090,1.);
#1738=VECTOR('',#6091,1.);
#1739=VECTOR('',#6094,1.);
#1740=VECTOR('',#6095,1.);
#1741=VECTOR('',#6096,1.);
#1742=VECTOR('',#6099,1.);
#1743=VECTOR('',#6102,1.);
#1744=VECTOR('',#6103,1.);
#1745=VECTOR('',#6106,1.);
#1746=VECTOR('',#6107,1.);
#1747=VECTOR('',#6108,1.);
#1748=VECTOR('',#6111,1.);
#1749=VECTOR('',#6112,1.);
#1750=VECTOR('',#6115,1.);
#1751=VECTOR('',#6122,0.5);
#1752=VECTOR('',#6125,1.);
#1753=VECTOR('',#6128,1.);
#1754=VECTOR('',#6131,1.);
#1755=VECTOR('',#6134,1.);
#1756=VECTOR('',#6141,0.305);
#1757=VECTOR('',#6146,1.);
#1758=VECTOR('',#6147,1.);
#1759=VECTOR('',#6148,1.);
#1760=VECTOR('',#6149,1.);
#1761=VECTOR('',#6152,1.);
#1762=VECTOR('',#6153,1.);
#1763=VECTOR('',#6154,1.);
#1764=VECTOR('',#6155,1.);
#1765=VECTOR('',#6158,1.);
#1766=VECTOR('',#6159,1.);
#1767=VECTOR('',#6160,1.);
#1768=VECTOR('',#6163,1.);
#1769=VECTOR('',#6164,1.);
#1770=VECTOR('',#6167,1.);
#1771=VECTOR('',#6168,1.);
#1772=VECTOR('',#6171,1.);
#1773=VECTOR('',#6172,1.);
#1774=VECTOR('',#6173,1.);
#1775=VECTOR('',#6174,1.);
#1776=VECTOR('',#6177,1.);
#1777=VECTOR('',#6178,1.);
#1778=VECTOR('',#6179,1.);
#1779=VECTOR('',#6182,1.);
#1780=VECTOR('',#6183,1.);
#1781=VECTOR('',#6186,1.);
#1782=VECTOR('',#6187,1.);
#1783=VECTOR('',#6196,0.305);
#1784=VECTOR('',#6201,1.);
#1785=VECTOR('',#6202,1.);
#1786=VECTOR('',#6203,1.);
#1787=VECTOR('',#6204,1.);
#1788=VECTOR('',#6205,1.);
#1789=VECTOR('',#6206,1.);
#1790=VECTOR('',#6209,1.);
#1791=VECTOR('',#6210,1.);
#1792=VECTOR('',#6211,1.);
#1793=VECTOR('',#6214,1.);
#1794=VECTOR('',#6215,1.);
#1795=VECTOR('',#6216,1.);
#1796=VECTOR('',#6219,1.);
#1797=VECTOR('',#6220,1.);
#1798=VECTOR('',#6223,1.);
#1799=VECTOR('',#6226,1.);
#1800=VECTOR('',#6227,1.);
#1801=VECTOR('',#6228,1.);
#1802=VECTOR('',#6229,1.);
#1803=VECTOR('',#6232,1.);
#1804=VECTOR('',#6233,1.);
#1805=VECTOR('',#6234,1.);
#1806=VECTOR('',#6237,1.);
#1807=VECTOR('',#6240,1.);
#1808=VECTOR('',#6241,1.);
#1809=VECTOR('',#6244,1.);
#1810=VECTOR('',#6251,0.275);
#1811=VECTOR('',#6256,0.275);
#1812=VECTOR('',#6261,0.275);
#1813=VECTOR('',#6266,0.275);
#1814=VECTOR('',#6277,0.7);
#1815=VECTOR('',#6282,0.5);
#1816=VECTOR('',#6289,1.);
#1817=VECTOR('',#6290,1.);
#1818=VECTOR('',#6291,1.);
#1819=VECTOR('',#6292,1.);
#1820=VECTOR('',#6295,1.);
#1821=VECTOR('',#6296,1.);
#1822=VECTOR('',#6297,1.);
#1823=VECTOR('',#6300,1.);
#1824=VECTOR('',#6301,1.);
#1825=VECTOR('',#6302,1.);
#1826=VECTOR('',#6305,1.);
#1827=VECTOR('',#6306,1.);
#1828=VECTOR('',#6325,1.);
#1829=VECTOR('',#6326,1.);
#1830=VECTOR('',#6327,1.);
#1831=VECTOR('',#6328,1.);
#1832=VECTOR('',#6331,1.);
#1833=VECTOR('',#6332,1.);
#1834=VECTOR('',#6333,1.);
#1835=VECTOR('',#6336,1.);
#1836=VECTOR('',#6337,1.);
#1837=VECTOR('',#6338,1.);
#1838=VECTOR('',#6341,1.);
#1839=VECTOR('',#6342,1.);
#1840=VECTOR('',#6343,1.);
#1841=VECTOR('',#6346,1.);
#1842=VECTOR('',#6347,1.);
#1843=VECTOR('',#6348,1.);
#1844=VECTOR('',#6351,1.);
#1845=VECTOR('',#6352,1.);
#1846=VECTOR('',#6369,0.4);
#1847=VECTOR('',#6374,0.425);
#1848=VECTOR('',#6379,0.41);
#1849=VECTOR('',#6388,0.26);
#1850=VECTOR('',#6391,0.25);
#1851=VECTOR('',#6420,0.165);
#1852=VECTOR('',#6429,0.165);
#1853=VECTOR('',#6438,0.165);
#1854=VECTOR('',#6447,0.165);
#1855=VECTOR('',#6456,0.165);
#1856=VECTOR('',#6465,0.165);
#1857=VECTOR('',#6474,0.165);
#1858=VECTOR('',#6483,0.165);
#1859=VECTOR('',#6492,0.25);
#1860=VECTOR('',#6499,1.);
#1861=VECTOR('',#6502,1.);
#1862=VECTOR('',#6507,1.);
#1863=VECTOR('',#6510,1.);
#1864=VECTOR('',#6513,1.);
#1865=VECTOR('',#6514,1.);
#1866=VECTOR('',#6517,1.);
#1867=VECTOR('',#6518,1.);
#1868=VECTOR('',#6527,1.5);
#1869=VECTOR('',#6534,2.2);
#1870=VECTOR('',#6547,1.02);
#1871=VECTOR('',#6554,1.49);
#1872=VECTOR('',#6567,0.505);
#1873=VECTOR('',#6574,0.7);
#1874=VECTOR('',#6587,0.375);
#1875=VECTOR('',#6598,0.375);
#1876=VECTOR('',#6609,0.375);
#1877=VECTOR('',#6620,0.375);
#1878=VECTOR('',#6629,0.225);
#1879=VECTOR('',#6634,0.225);
#1880=VECTOR('',#6639,0.225);
#1881=VECTOR('',#6644,0.225);
#1882=VECTOR('',#6651,1.49);
#1883=VECTOR('',#6660,0.71);
#1884=VECTOR('',#6667,2.2);
#1885=VECTOR('',#6680,0.375);
#1886=VECTOR('',#6691,0.375);
#1887=VECTOR('',#6702,0.375);
#1888=VECTOR('',#6713,0.375);
#1889=VECTOR('',#6724,0.225);
#1890=VECTOR('',#6729,0.225);
#1891=VECTOR('',#6734,0.225);
#1892=VECTOR('',#6739,0.225);
#1893=VECTOR('',#6742,1.);
#1894=VECTOR('',#6743,1.);
#1895=VECTOR('',#6744,1.);
#1896=VECTOR('',#6745,1.);
#1897=VECTOR('',#6748,1.);
#1898=VECTOR('',#6749,1.);
#1899=VECTOR('',#6750,1.);
#1900=VECTOR('',#6751,1.);
#1901=VECTOR('',#6754,1.);
#1902=VECTOR('',#6755,1.);
#1903=VECTOR('',#6760,1.49);
#1904=VECTOR('',#6771,0.71);
#1905=VECTOR('',#6788,0.300000000000001);
#1906=VECTOR('',#6797,1.2);
#1907=VECTOR('',#6810,1.2);
#1908=VECTOR('',#6835,0.976185);
#1909=VECTOR('',#6842,0.5);
#1910=VECTOR('',#6847,0.53);
#1911=VECTOR('',#6856,0.976185);
#1912=VECTOR('',#6863,0.53);
#1913=VECTOR('',#6882,1.023815);
#1914=VECTOR('',#6893,1.47);
#1915=VECTOR('',#6898,1.5);
#1916=VECTOR('',#6903,1.47);
#1917=VECTOR('',#6908,1.023815);
#1918=VECTOR('',#6959,1.019052);
#1919=VECTOR('',#7036,0.980948);
#1920=VECTOR('',#7065,1.013815);
#1921=VECTOR('',#7072,0.991185);
#1922=VECTOR('',#7083,1.013815);
#1923=VECTOR('',#7090,0.991185);
#1924=VECTOR('',#7109,0.165);
#1925=VECTOR('',#7118,0.165);
#1926=VECTOR('',#7131,0.5);
#1927=VECTOR('',#7144,0.5);
#1928=VECTOR('',#7147,0.3);
#1929=VECTOR('',#7154,0.3);
#1930=VECTOR('',#7163,1.2);
#1931=VECTOR('',#7176,0.225);
#1932=VECTOR('',#7181,1.);
#1933=VECTOR('',#7184,1.);
#1934=VECTOR('',#7189,1.);
#1935=VECTOR('',#7194,1.);
#1936=VECTOR('',#7199,1.);
#1937=VECTOR('',#7200,1.);
#1938=VECTOR('',#7203,1.);
#1939=VECTOR('',#7204,1.);
#1940=VECTOR('',#7213,0.3);
#1941=VECTOR('',#7218,0.7);
#1942=VECTOR('',#7227,0.164999999999999);
#1943=VECTOR('',#7236,0.6);
#1944=VECTOR('',#7249,0.225);
#1945=VECTOR('',#7256,0.6);
#1946=VECTOR('',#7269,0.225);
#1947=VECTOR('',#7276,0.6);
#1948=VECTOR('',#7293,0.325);
#1949=VECTOR('',#7298,0.35);
#1950=VECTOR('',#7303,0.335);
#1951=VECTOR('',#7312,0.21);
#1952=VECTOR('',#7317,0.2);
#1953=VECTOR('',#7322,0.18);
#1954=VECTOR('',#7327,1.);
#1955=VECTOR('',#7328,1.);
#1956=VECTOR('',#7329,1.);
#1957=VECTOR('',#7330,1.);
#1958=VECTOR('',#7333,1.);
#1959=VECTOR('',#7334,1.);
#1960=VECTOR('',#7335,1.);
#1961=VECTOR('',#7338,1.);
#1962=VECTOR('',#7339,1.);
#1963=VECTOR('',#7340,1.);
#1964=VECTOR('',#7343,1.);
#1965=VECTOR('',#7344,1.);
#1966=VECTOR('',#7345,1.);
#1967=VECTOR('',#7348,1.);
#1968=VECTOR('',#7349,1.);
#1969=VECTOR('',#7350,1.);
#1970=VECTOR('',#7353,1.);
#1971=VECTOR('',#7354,1.);
#1972=VECTOR('',#7363,1.);
#1973=VECTOR('',#7364,1.);
#1974=VECTOR('',#7365,1.);
#1975=VECTOR('',#7366,1.);
#1976=VECTOR('',#7369,1.);
#1977=VECTOR('',#7370,1.);
#1978=VECTOR('',#7371,1.);
#1979=VECTOR('',#7374,1.);
#1980=VECTOR('',#7375,1.);
#1981=VECTOR('',#7376,1.);
#1982=VECTOR('',#7379,1.);
#1983=VECTOR('',#7380,1.);
#1984=VECTOR('',#7381,1.);
#1985=VECTOR('',#7384,1.);
#1986=VECTOR('',#7385,1.);
#1987=VECTOR('',#7386,1.);
#1988=VECTOR('',#7389,1.);
#1989=VECTOR('',#7390,1.);
#1990=VECTOR('',#7407,0.325);
#1991=VECTOR('',#7412,0.35);
#1992=VECTOR('',#7417,0.335);
#1993=VECTOR('',#7426,0.21);
#1994=VECTOR('',#7429,0.2);
#1995=CIRCLE('',#5227,0.21);
#1996=CIRCLE('',#5228,0.21);
#1997=CIRCLE('',#5230,0.21);
#1998=CIRCLE('',#5231,0.21);
#1999=CIRCLE('',#5233,0.21);
#2000=CIRCLE('',#5234,0.21);
#2001=CIRCLE('',#5236,0.21);
#2002=CIRCLE('',#5237,0.21);
#2003=CIRCLE('',#5260,1.8);
#2004=CIRCLE('',#5261,0.5);
#2005=CIRCLE('',#5262,0.275);
#2006=CIRCLE('',#5264,0.5);
#2007=CIRCLE('',#5266,1.8);
#2008=CIRCLE('',#5267,0.5);
#2009=CIRCLE('',#5268,0.275);
#2010=CIRCLE('',#5270,0.5);
#2011=CIRCLE('',#5272,1.8);
#2012=CIRCLE('',#5273,0.5);
#2013=CIRCLE('',#5274,0.275);
#2014=CIRCLE('',#5276,0.5);
#2015=CIRCLE('',#5278,1.8);
#2016=CIRCLE('',#5279,0.5);
#2017=CIRCLE('',#5280,0.275);
#2018=CIRCLE('',#5282,0.5);
#2019=CIRCLE('',#5284,1.8);
#2020=CIRCLE('',#5285,1.8);
#2021=CIRCLE('',#5286,1.8);
#2022=CIRCLE('',#5287,1.8);
#2023=CIRCLE('',#5288,1.8);
#2024=CIRCLE('',#5289,0.5);
#2025=CIRCLE('',#5291,1.8);
#2026=CIRCLE('',#5293,0.3);
#2027=CIRCLE('',#5294,0.3);
#2028=CIRCLE('',#5302,0.5);
#2029=CIRCLE('',#5308,0.5);
#2030=CIRCLE('',#5310,0.5);
#2031=CIRCLE('',#5311,0.5);
#2032=CIRCLE('',#5312,0.5);
#2033=CIRCLE('',#5313,0.5);
#2034=CIRCLE('',#5314,0.5);
#2035=CIRCLE('',#5316,0.305);
#2036=CIRCLE('',#5317,0.305);
#2037=CIRCLE('',#5330,0.305);
#2038=CIRCLE('',#5331,0.305);
#2039=CIRCLE('',#5344,0.275);
#2040=CIRCLE('',#5346,0.275);
#2041=CIRCLE('',#5348,0.275);
#2042=CIRCLE('',#5350,0.275);
#2043=CIRCLE('',#5352,0.7);
#2044=CIRCLE('',#5353,0.5);
#2045=CIRCLE('',#5355,0.7);
#2046=CIRCLE('',#5367,0.075);
#2047=CIRCLE('',#5368,0.075);
#2048=CIRCLE('',#5381,0.24505);
#2049=CIRCLE('',#5383,0.375);
#2050=CIRCLE('',#5385,0.425);
#2051=CIRCLE('',#5387,0.425);
#2052=CIRCLE('',#5389,0.395);
#2053=CIRCLE('',#5391,0.27);
#2054=CIRCLE('',#5393,0.24505);
#2055=CIRCLE('',#5408,0.165);
#2056=CIRCLE('',#5409,0.165);
#2057=CIRCLE('',#5412,0.165);
#2058=CIRCLE('',#5413,0.165);
#2059=CIRCLE('',#5416,0.165);
#2060=CIRCLE('',#5417,0.165);
#2061=CIRCLE('',#5420,0.165);
#2062=CIRCLE('',#5421,0.165);
#2063=CIRCLE('',#5424,0.165);
#2064=CIRCLE('',#5425,0.165);
#2065=CIRCLE('',#5428,0.165);
#2066=CIRCLE('',#5429,0.165);
#2067=CIRCLE('',#5432,0.165);
#2068=CIRCLE('',#5433,0.165);
#2069=CIRCLE('',#5436,0.165);
#2070=CIRCLE('',#5437,0.165);
#2071=CIRCLE('',#5440,0.25);
#2072=CIRCLE('',#5441,0.25);
#2073=CIRCLE('',#5444,1.4);
#2074=CIRCLE('',#5445,1.4);
#2075=CIRCLE('',#5447,2.2);
#2076=CIRCLE('',#5451,2.2);
#2077=CIRCLE('',#5453,1.5);
#2078=CIRCLE('',#5454,1.5);
#2079=CIRCLE('',#5456,2.2);
#2080=CIRCLE('',#5457,2.2);
#2081=CIRCLE('',#5462,1.02);
#2082=CIRCLE('',#5463,1.02);
#2083=CIRCLE('',#5465,1.49);
#2084=CIRCLE('',#5466,1.49);
#2085=CIRCLE('',#5471,0.505);
#2086=CIRCLE('',#5472,0.505);
#2087=CIRCLE('',#5474,0.7);
#2088=CIRCLE('',#5475,0.7);
#2089=CIRCLE('',#5480,0.375);
#2090=CIRCLE('',#5481,0.375);
#2091=CIRCLE('',#5483,0.225);
#2092=CIRCLE('',#5485,0.375);
#2093=CIRCLE('',#5486,0.375);
#2094=CIRCLE('',#5488,0.225);
#2095=CIRCLE('',#5490,0.375);
#2096=CIRCLE('',#5491,0.375);
#2097=CIRCLE('',#5493,0.225);
#2098=CIRCLE('',#5495,0.375);
#2099=CIRCLE('',#5496,0.375);
#2100=CIRCLE('',#5498,0.225);
#2101=CIRCLE('',#5500,0.225);
#2102=CIRCLE('',#5502,0.225);
#2103=CIRCLE('',#5504,0.225);
#2104=CIRCLE('',#5506,0.225);
#2105=CIRCLE('',#5508,1.49);
#2106=CIRCLE('',#5509,1.49);
#2107=CIRCLE('',#5511,0.71);
#2108=CIRCLE('',#5513,0.71);
#2109=CIRCLE('',#5515,2.2);
#2110=CIRCLE('',#5516,2.2);
#2111=CIRCLE('',#5521,0.375);
#2112=CIRCLE('',#5522,0.375);
#2113=CIRCLE('',#5524,0.225);
#2114=CIRCLE('',#5526,0.375);
#2115=CIRCLE('',#5527,0.375);
#2116=CIRCLE('',#5529,0.225);
#2117=CIRCLE('',#5531,0.375);
#2118=CIRCLE('',#5532,0.375);
#2119=CIRCLE('',#5534,0.225);
#2120=CIRCLE('',#5536,0.375);
#2121=CIRCLE('',#5537,0.375);
#2122=CIRCLE('',#5539,0.225);
#2123=CIRCLE('',#5541,0.225);
#2124=CIRCLE('',#5543,0.225);
#2125=CIRCLE('',#5545,0.225);
#2126=CIRCLE('',#5547,0.225);
#2127=CIRCLE('',#5552,1.49);
#2128=CIRCLE('',#5553,1.49);
#2129=CIRCLE('',#5555,0.71);
#2130=CIRCLE('',#5557,0.71);
#2131=CIRCLE('',#5559,2.2);
#2132=CIRCLE('',#5560,2.2);
#2133=CIRCLE('',#5565,0.300000000000001);
#2134=CIRCLE('',#5566,0.300000000000001);
#2135=CIRCLE('',#5569,1.2);
#2136=CIRCLE('',#5570,1.2);
#2137=CIRCLE('',#5575,1.2);
#2138=CIRCLE('',#5576,1.2);
#2139=CIRCLE('',#5582,0.976185);
#2140=CIRCLE('',#5583,0.976185);
#2141=CIRCLE('',#5584,0.247676);
#2142=CIRCLE('',#5585,0.976185);
#2143=CIRCLE('',#5586,0.976185);
#2144=CIRCLE('',#5588,0.976185);
#2145=CIRCLE('',#5590,0.5);
#2146=CIRCLE('',#5591,0.5);
#2147=CIRCLE('',#5593,0.56);
#2148=CIRCLE('',#5596,0.976185);
#2149=CIRCLE('',#5598,0.56);
#2150=CIRCLE('',#5602,1.023815);
#2151=CIRCLE('',#5603,1.023815);
#2152=CIRCLE('',#5604,0.247676);
#2153=CIRCLE('',#5605,1.023815);
#2154=CIRCLE('',#5606,1.023815);
#2155=CIRCLE('',#5608,1.023815);
#2156=CIRCLE('',#5610,1.44);
#2157=CIRCLE('',#5611,1.023815);
#2158=CIRCLE('',#5613,1.5);
#2159=CIRCLE('',#5615,1.5);
#2160=CIRCLE('',#5617,1.44);
#2161=CIRCLE('',#5622,0.23815);
#2162=CIRCLE('',#5624,0.23815);
#2163=CIRCLE('',#5626,0.23815);
#2164=CIRCLE('',#5628,0.23815);
#2165=CIRCLE('',#5630,0.23815);
#2166=CIRCLE('',#5632,0.23815);
#2167=CIRCLE('',#5634,0.23815);
#2168=CIRCLE('',#5636,0.23815);
#2169=CIRCLE('',#5639,0.243053047864041);
#2170=CIRCLE('',#5640,0.243053047864041);
#2171=CIRCLE('',#5642,1.019052);
#2172=CIRCLE('',#5643,1.019052);
#2173=CIRCLE('',#5644,1.019052);
#2174=CIRCLE('',#5645,1.019052);
#2175=CIRCLE('',#5646,1.019052);
#2176=CIRCLE('',#5647,1.019052);
#2177=CIRCLE('',#5648,1.019052);
#2178=CIRCLE('',#5649,1.019052);
#2179=CIRCLE('',#5650,1.019052);
#2180=CIRCLE('',#5652,0.980948);
#2181=CIRCLE('',#5653,0.243053047864041);
#2182=CIRCLE('',#5655,0.243053047864041);
#2183=CIRCLE('',#5657,0.980948);
#2184=CIRCLE('',#5658,0.243053047864041);
#2185=CIRCLE('',#5660,0.243053047864041);
#2186=CIRCLE('',#5662,0.980948);
#2187=CIRCLE('',#5663,0.243053047864041);
#2188=CIRCLE('',#5665,0.243053047864041);
#2189=CIRCLE('',#5667,0.980948);
#2190=CIRCLE('',#5668,0.243053047864041);
#2191=CIRCLE('',#5670,0.243053047864041);
#2192=CIRCLE('',#5672,0.980948);
#2193=CIRCLE('',#5673,0.243053047864041);
#2194=CIRCLE('',#5675,0.243053047864041);
#2195=CIRCLE('',#5677,0.980948);
#2196=CIRCLE('',#5678,0.243053047864041);
#2197=CIRCLE('',#5680,0.243053047864041);
#2198=CIRCLE('',#5682,0.980948);
#2199=CIRCLE('',#5683,0.980948);
#2200=CIRCLE('',#5684,0.980948);
#2201=CIRCLE('',#5686,0.243053047864041);
#2202=CIRCLE('',#5688,0.243053047864041);
#2203=CIRCLE('',#5693,1.013815);
#2204=CIRCLE('',#5694,0.991185);
#2205=CIRCLE('',#5696,1.013815);
#2206=CIRCLE('',#5698,0.991185);
#2207=CIRCLE('',#5701,1.013815);
#2208=CIRCLE('',#5702,0.991185);
#2209=CIRCLE('',#5704,1.013815);
#2210=CIRCLE('',#5706,0.991185);
#2211=CIRCLE('',#5716,0.165);
#2212=CIRCLE('',#5717,0.165);
#2213=CIRCLE('',#5720,0.165);
#2214=CIRCLE('',#5721,0.165);
#2215=CIRCLE('',#5724,0.5);
#2216=CIRCLE('',#5725,0.3);
#2217=CIRCLE('',#5727,0.5);
#2218=CIRCLE('',#5729,0.5);
#2219=CIRCLE('',#5730,0.3);
#2220=CIRCLE('',#5732,0.5);
#2221=CIRCLE('',#5734,0.3);
#2222=CIRCLE('',#5736,0.3);
#2223=CIRCLE('',#5740,1.2);
#2224=CIRCLE('',#5741,1.2);
#2225=CIRCLE('',#5746,0.225);
#2226=CIRCLE('',#5747,0.225);
#2227=CIRCLE('',#5749,0.699999999999999);
#2228=CIRCLE('',#5750,0.699999999999999);
#2229=CIRCLE('',#5752,0.7);
#2230=CIRCLE('',#5753,0.7);
#2231=CIRCLE('',#5754,0.3);
#2232=CIRCLE('',#5758,0.7);
#2233=CIRCLE('',#5760,0.3);
#2234=CIRCLE('',#5762,0.7);
#2235=CIRCLE('',#5766,0.164999999999999);
#2236=CIRCLE('',#5767,0.164999999999999);
#2237=CIRCLE('',#5770,0.6);
#2238=CIRCLE('',#5771,0.6);
#2239=CIRCLE('',#5776,0.225);
#2240=CIRCLE('',#5777,0.225);
#2241=CIRCLE('',#5779,0.6);
#2242=CIRCLE('',#5780,0.6);
#2243=CIRCLE('',#5785,0.225);
#2244=CIRCLE('',#5786,0.225);
#2245=CIRCLE('',#5788,0.6);
#2246=CIRCLE('',#5789,0.6);
#2247=CIRCLE('',#5794,0.3);
#2248=CIRCLE('',#5796,0.35);
#2249=CIRCLE('',#5798,0.35);
#2250=CIRCLE('',#5800,0.32);
#2251=CIRCLE('',#5802,0.22);
#2252=CIRCLE('',#5804,0.1954);
#2253=CIRCLE('',#5806,0.1954);
#2254=CIRCLE('',#5808,0.16);
#2255=CIRCLE('',#5828,0.1954);
#2256=CIRCLE('',#5830,0.3);
#2257=CIRCLE('',#5832,0.35);
#2258=CIRCLE('',#5834,0.35);
#2259=CIRCLE('',#5836,0.32);
#2260=CIRCLE('',#5838,0.22);
#2261=CIRCLE('',#5840,0.1954);
#2262=VERTEX_POINT('',#7490);
#2263=VERTEX_POINT('',#7492);
#2264=VERTEX_POINT('',#7496);
#2265=VERTEX_POINT('',#7498);
#2266=VERTEX_POINT('',#7502);
#2267=VERTEX_POINT('',#7504);
#2268=VERTEX_POINT('',#7508);
#2269=VERTEX_POINT('',#7510);
#2270=VERTEX_POINT('',#7514);
#2271=VERTEX_POINT('',#7515);
#2272=VERTEX_POINT('',#7517);
#2273=VERTEX_POINT('',#7519);
#2274=VERTEX_POINT('',#7523);
#2275=VERTEX_POINT('',#7525);
#2276=VERTEX_POINT('',#7529);
#2277=VERTEX_POINT('',#7531);
#2278=VERTEX_POINT('',#7541);
#2279=VERTEX_POINT('',#7542);
#2280=VERTEX_POINT('',#7544);
#2281=VERTEX_POINT('',#7546);
#2282=VERTEX_POINT('',#7550);
#2283=VERTEX_POINT('',#7552);
#2284=VERTEX_POINT('',#7556);
#2285=VERTEX_POINT('',#7558);
#2286=VERTEX_POINT('',#7568);
#2287=VERTEX_POINT('',#7569);
#2288=VERTEX_POINT('',#7571);
#2289=VERTEX_POINT('',#7573);
#2290=VERTEX_POINT('',#7577);
#2291=VERTEX_POINT('',#7579);
#2292=VERTEX_POINT('',#7583);
#2293=VERTEX_POINT('',#7585);
#2294=VERTEX_POINT('',#7595);
#2295=VERTEX_POINT('',#7596);
#2296=VERTEX_POINT('',#7599);
#2297=VERTEX_POINT('',#7602);
#2298=VERTEX_POINT('',#7604);
#2299=VERTEX_POINT('',#7608);
#2300=VERTEX_POINT('',#7609);
#2301=VERTEX_POINT('',#7612);
#2302=VERTEX_POINT('',#7615);
#2303=VERTEX_POINT('',#7617);
#2304=VERTEX_POINT('',#7621);
#2305=VERTEX_POINT('',#7622);
#2306=VERTEX_POINT('',#7625);
#2307=VERTEX_POINT('',#7628);
#2308=VERTEX_POINT('',#7630);
#2309=VERTEX_POINT('',#7634);
#2310=VERTEX_POINT('',#7635);
#2311=VERTEX_POINT('',#7638);
#2312=VERTEX_POINT('',#7641);
#2313=VERTEX_POINT('',#7643);
#2314=VERTEX_POINT('',#7650);
#2315=VERTEX_POINT('',#7653);
#2316=VERTEX_POINT('',#7656);
#2317=VERTEX_POINT('',#7660);
#2318=VERTEX_POINT('',#7662);
#2319=VERTEX_POINT('',#7667);
#2320=VERTEX_POINT('',#7668);
#2321=VERTEX_POINT('',#7670);
#2322=VERTEX_POINT('',#7672);
#2323=VERTEX_POINT('',#7674);
#2324=VERTEX_POINT('',#7676);
#2325=VERTEX_POINT('',#7680);
#2326=VERTEX_POINT('',#7682);
#2327=VERTEX_POINT('',#7686);
#2328=VERTEX_POINT('',#7687);
#2329=VERTEX_POINT('',#7694);
#2330=VERTEX_POINT('',#7696);
#2331=VERTEX_POINT('',#7700);
#2332=VERTEX_POINT('',#7702);
#2333=VERTEX_POINT('',#7704);
#2334=VERTEX_POINT('',#7706);
#2335=VERTEX_POINT('',#7710);
#2336=VERTEX_POINT('',#7714);
#2337=VERTEX_POINT('',#7716);
#2338=VERTEX_POINT('',#7720);
#2339=VERTEX_POINT('',#7728);
#2340=VERTEX_POINT('',#7731);
#2341=VERTEX_POINT('',#7732);
#2342=VERTEX_POINT('',#7734);
#2343=VERTEX_POINT('',#7736);
#2344=VERTEX_POINT('',#7739);
#2345=VERTEX_POINT('',#7740);
#2346=VERTEX_POINT('',#7742);
#2347=VERTEX_POINT('',#7744);
#2348=VERTEX_POINT('',#7748);
#2349=VERTEX_POINT('',#7750);
#2350=VERTEX_POINT('',#7754);
#2351=VERTEX_POINT('',#7755);
#2352=VERTEX_POINT('',#7757);
#2353=VERTEX_POINT('',#7759);
#2354=VERTEX_POINT('',#7763);
#2355=VERTEX_POINT('',#7764);
#2356=VERTEX_POINT('',#7766);
#2357=VERTEX_POINT('',#7768);
#2358=VERTEX_POINT('',#7772);
#2359=VERTEX_POINT('',#7774);
#2360=VERTEX_POINT('',#7781);
#2361=VERTEX_POINT('',#7785);
#2362=VERTEX_POINT('',#7788);
#2363=VERTEX_POINT('',#7792);
#2364=VERTEX_POINT('',#7794);
#2365=VERTEX_POINT('',#7798);
#2366=VERTEX_POINT('',#7807);
#2367=VERTEX_POINT('',#7809);
#2368=VERTEX_POINT('',#7813);
#2369=VERTEX_POINT('',#7814);
#2370=VERTEX_POINT('',#7816);
#2371=VERTEX_POINT('',#7818);
#2372=VERTEX_POINT('',#7820);
#2373=VERTEX_POINT('',#7822);
#2374=VERTEX_POINT('',#7826);
#2375=VERTEX_POINT('',#7828);
#2376=VERTEX_POINT('',#7832);
#2377=VERTEX_POINT('',#7834);
#2378=VERTEX_POINT('',#7838);
#2379=VERTEX_POINT('',#7844);
#2380=VERTEX_POINT('',#7846);
#2381=VERTEX_POINT('',#7848);
#2382=VERTEX_POINT('',#7853);
#2383=VERTEX_POINT('',#7859);
#2384=VERTEX_POINT('',#7866);
#2385=VERTEX_POINT('',#7870);
#2386=VERTEX_POINT('',#7874);
#2387=VERTEX_POINT('',#7878);
#2388=VERTEX_POINT('',#7882);
#2389=VERTEX_POINT('',#7884);
#2390=VERTEX_POINT('',#7887);
#2391=VERTEX_POINT('',#7896);
#2392=VERTEX_POINT('',#7897);
#2393=VERTEX_POINT('',#7899);
#2394=VERTEX_POINT('',#7901);
#2395=VERTEX_POINT('',#7905);
#2396=VERTEX_POINT('',#7907);
#2397=VERTEX_POINT('',#7911);
#2398=VERTEX_POINT('',#7913);
#2399=VERTEX_POINT('',#9142);
#2400=VERTEX_POINT('',#9144);
#2401=VERTEX_POINT('',#9272);
#2402=VERTEX_POINT('',#9273);
#2403=VERTEX_POINT('',#9275);
#2404=VERTEX_POINT('',#9277);
#2405=VERTEX_POINT('',#9281);
#2406=VERTEX_POINT('',#9283);
#2407=VERTEX_POINT('',#9287);
#2408=VERTEX_POINT('',#9289);
#2409=VERTEX_POINT('',#9293);
#2410=VERTEX_POINT('',#9295);
#2411=VERTEX_POINT('',#9299);
#2412=VERTEX_POINT('',#9301);
#2413=VERTEX_POINT('',#9310);
#2414=VERTEX_POINT('',#9313);
#2415=VERTEX_POINT('',#9316);
#2416=VERTEX_POINT('',#9320);
#2417=VERTEX_POINT('',#9324);
#2418=VERTEX_POINT('',#9328);
#2419=VERTEX_POINT('',#9331);
#2420=VERTEX_POINT('',#9349);
#2421=VERTEX_POINT('',#9351);
#2422=VERTEX_POINT('',#9356);
#2423=VERTEX_POINT('',#9358);
#2424=VERTEX_POINT('',#9363);
#2425=VERTEX_POINT('',#9365);
#2426=VERTEX_POINT('',#9370);
#2427=VERTEX_POINT('',#9372);
#2428=VERTEX_POINT('',#9377);
#2429=VERTEX_POINT('',#9379);
#2430=VERTEX_POINT('',#9384);
#2431=VERTEX_POINT('',#9386);
#2432=VERTEX_POINT('',#9391);
#2433=VERTEX_POINT('',#9393);
#2434=VERTEX_POINT('',#9398);
#2435=VERTEX_POINT('',#9400);
#2436=VERTEX_POINT('',#9405);
#2437=VERTEX_POINT('',#9407);
#2438=VERTEX_POINT('',#9412);
#2439=VERTEX_POINT('',#9413);
#2440=VERTEX_POINT('',#9415);
#2441=VERTEX_POINT('',#9417);
#2442=VERTEX_POINT('',#9421);
#2443=VERTEX_POINT('',#9423);
#2444=VERTEX_POINT('',#9427);
#2445=VERTEX_POINT('',#9431);
#2446=VERTEX_POINT('',#9437);
#2447=VERTEX_POINT('',#9439);
#2448=VERTEX_POINT('',#9443);
#2449=VERTEX_POINT('',#9445);
#2450=VERTEX_POINT('',#9452);
#2451=VERTEX_POINT('',#9454);
#2452=VERTEX_POINT('',#9458);
#2453=VERTEX_POINT('',#9460);
#2454=VERTEX_POINT('',#9467);
#2455=VERTEX_POINT('',#9469);
#2456=VERTEX_POINT('',#9473);
#2457=VERTEX_POINT('',#9475);
#2458=VERTEX_POINT('',#9482);
#2459=VERTEX_POINT('',#9484);
#2460=VERTEX_POINT('',#9488);
#2461=VERTEX_POINT('',#9491);
#2462=VERTEX_POINT('',#9493);
#2463=VERTEX_POINT('',#9497);
#2464=VERTEX_POINT('',#9500);
#2465=VERTEX_POINT('',#9502);
#2466=VERTEX_POINT('',#9506);
#2467=VERTEX_POINT('',#9509);
#2468=VERTEX_POINT('',#9511);
#2469=VERTEX_POINT('',#9515);
#2470=VERTEX_POINT('',#9518);
#2471=VERTEX_POINT('',#9522);
#2472=VERTEX_POINT('',#9526);
#2473=VERTEX_POINT('',#9530);
#2474=VERTEX_POINT('',#9534);
#2475=VERTEX_POINT('',#9536);
#2476=VERTEX_POINT('',#9540);
#2477=VERTEX_POINT('',#9543);
#2478=VERTEX_POINT('',#9547);
#2479=VERTEX_POINT('',#9549);
#2480=VERTEX_POINT('',#9556);
#2481=VERTEX_POINT('',#9558);
#2482=VERTEX_POINT('',#9562);
#2483=VERTEX_POINT('',#9565);
#2484=VERTEX_POINT('',#9567);
#2485=VERTEX_POINT('',#9571);
#2486=VERTEX_POINT('',#9574);
#2487=VERTEX_POINT('',#9576);
#2488=VERTEX_POINT('',#9580);
#2489=VERTEX_POINT('',#9583);
#2490=VERTEX_POINT('',#9585);
#2491=VERTEX_POINT('',#9589);
#2492=VERTEX_POINT('',#9592);
#2493=VERTEX_POINT('',#9596);
#2494=VERTEX_POINT('',#9600);
#2495=VERTEX_POINT('',#9604);
#2496=VERTEX_POINT('',#9608);
#2497=VERTEX_POINT('',#9609);
#2498=VERTEX_POINT('',#9611);
#2499=VERTEX_POINT('',#9613);
#2500=VERTEX_POINT('',#9617);
#2501=VERTEX_POINT('',#9618);
#2502=VERTEX_POINT('',#9620);
#2503=VERTEX_POINT('',#9622);
#2504=VERTEX_POINT('',#9629);
#2505=VERTEX_POINT('',#9631);
#2506=VERTEX_POINT('',#9635);
#2507=VERTEX_POINT('',#9638);
#2508=VERTEX_POINT('',#9648);
#2509=VERTEX_POINT('',#9650);
#2510=VERTEX_POINT('',#9655);
#2511=VERTEX_POINT('',#9657);
#2512=VERTEX_POINT('',#9664);
#2513=VERTEX_POINT('',#9666);
#2514=VERTEX_POINT('',#9674);
#2515=VERTEX_POINT('',#9675);
#2516=VERTEX_POINT('',#9678);
#2517=VERTEX_POINT('',#9680);
#2518=VERTEX_POINT('',#9684);
#2519=VERTEX_POINT('',#9688);
#2520=VERTEX_POINT('',#9690);
#2521=VERTEX_POINT('',#9694);
#2522=VERTEX_POINT('',#9699);
#2523=VERTEX_POINT('',#9703);
#2524=VERTEX_POINT('',#9709);
#2525=VERTEX_POINT('',#9710);
#2526=VERTEX_POINT('',#9713);
#2527=VERTEX_POINT('',#9715);
#2528=VERTEX_POINT('',#9719);
#2529=VERTEX_POINT('',#9723);
#2530=VERTEX_POINT('',#9725);
#2531=VERTEX_POINT('',#9728);
#2532=VERTEX_POINT('',#9732);
#2533=VERTEX_POINT('',#9736);
#2534=VERTEX_POINT('',#9744);
#2535=VERTEX_POINT('',#9745);
#2536=VERTEX_POINT('',#9748);
#2537=VERTEX_POINT('',#9749);
#2538=VERTEX_POINT('',#9752);
#2539=VERTEX_POINT('',#9753);
#2540=VERTEX_POINT('',#9756);
#2541=VERTEX_POINT('',#9757);
#2542=VERTEX_POINT('',#9760);
#2543=VERTEX_POINT('',#9761);
#2544=VERTEX_POINT('',#9764);
#2545=VERTEX_POINT('',#9765);
#2546=VERTEX_POINT('',#9768);
#2547=VERTEX_POINT('',#9769);
#2548=VERTEX_POINT('',#9772);
#2549=VERTEX_POINT('',#9773);
#2550=VERTEX_POINT('',#9777);
#2551=VERTEX_POINT('',#9778);
#2552=VERTEX_POINT('',#9801);
#2553=VERTEX_POINT('',#9803);
#2554=VERTEX_POINT('',#9828);
#2555=VERTEX_POINT('',#9830);
#2556=VERTEX_POINT('',#9853);
#2557=VERTEX_POINT('',#9855);
#2558=VERTEX_POINT('',#9878);
#2559=VERTEX_POINT('',#9880);
#2560=VERTEX_POINT('',#9893);
#2561=VERTEX_POINT('',#9896);
#2562=VERTEX_POINT('',#9909);
#2563=VERTEX_POINT('',#9911);
#2564=VERTEX_POINT('',#9934);
#2565=VERTEX_POINT('',#9936);
#2566=VERTEX_POINT('',#9959);
#2567=VERTEX_POINT('',#9961);
#2568=VERTEX_POINT('',#9984);
#2569=VERTEX_POINT('',#9986);
#2570=VERTEX_POINT('',#10011);
#2571=VERTEX_POINT('',#10015);
#2572=VERTEX_POINT('',#10040);
#2573=VERTEX_POINT('',#10044);
#2574=VERTEX_POINT('',#10069);
#2575=VERTEX_POINT('',#10073);
#2576=VERTEX_POINT('',#10074);
#2577=VERTEX_POINT('',#10101);
#2578=VERTEX_POINT('',#10105);
#2579=VERTEX_POINT('',#10130);
#2580=VERTEX_POINT('',#10134);
#2581=VERTEX_POINT('',#10159);
#2582=VERTEX_POINT('',#10163);
#2583=VERTEX_POINT('',#10188);
#2584=VERTEX_POINT('',#10191);
#2585=VERTEX_POINT('',#10193);
#2586=VERTEX_POINT('',#10225);
#2587=VERTEX_POINT('',#10227);
#2588=VERTEX_POINT('',#10230);
#2589=VERTEX_POINT('',#10234);
#2590=VERTEX_POINT('',#10239);
#2591=VERTEX_POINT('',#10241);
#2592=VERTEX_POINT('',#10244);
#2593=VERTEX_POINT('',#10248);
#2594=VERTEX_POINT('',#10260);
#2595=VERTEX_POINT('',#10262);
#2596=VERTEX_POINT('',#10267);
#2597=VERTEX_POINT('',#10269);
#2598=VERTEX_POINT('',#10274);
#2599=VERTEX_POINT('',#10276);
#2600=VERTEX_POINT('',#10279);
#2601=VERTEX_POINT('',#10283);
#2602=VERTEX_POINT('',#10285);
#2603=VERTEX_POINT('',#10288);
#2604=VERTEX_POINT('',#10292);
#2605=VERTEX_POINT('',#10296);
#2606=VERTEX_POINT('',#10302);
#2607=VERTEX_POINT('',#10304);
#2608=VERTEX_POINT('',#10311);
#2609=VERTEX_POINT('',#10313);
#2610=VERTEX_POINT('',#10317);
#2611=VERTEX_POINT('',#10318);
#2612=VERTEX_POINT('',#10320);
#2613=VERTEX_POINT('',#10322);
#2614=VERTEX_POINT('',#10326);
#2615=VERTEX_POINT('',#10328);
#2616=VERTEX_POINT('',#10330);
#2617=VERTEX_POINT('',#10333);
#2618=VERTEX_POINT('',#10336);
#2619=VERTEX_POINT('',#10340);
#2620=VERTEX_POINT('',#10346);
#2621=VERTEX_POINT('',#10350);
#2622=VERTEX_POINT('',#10356);
#2623=VERTEX_POINT('',#10358);
#2624=VERTEX_POINT('',#10363);
#2625=VERTEX_POINT('',#10365);
#2626=VERTEX_POINT('',#10372);
#2627=VERTEX_POINT('',#10374);
#2628=VERTEX_POINT('',#10378);
#2629=VERTEX_POINT('',#10380);
#2630=VERTEX_POINT('',#10387);
#2631=VERTEX_POINT('',#10389);
#2632=VERTEX_POINT('',#10393);
#2633=VERTEX_POINT('',#10395);
#2634=VERTEX_POINT('',#10402);
#2635=VERTEX_POINT('',#10405);
#2636=VERTEX_POINT('',#10409);
#2637=VERTEX_POINT('',#10413);
#2638=VERTEX_POINT('',#10417);
#2639=VERTEX_POINT('',#10420);
#2640=VERTEX_POINT('',#10424);
#2641=VERTEX_POINT('',#10428);
#2642=VERTEX_POINT('',#10433);
#2643=VERTEX_POINT('',#10434);
#2644=VERTEX_POINT('',#10436);
#2645=VERTEX_POINT('',#10438);
#2646=VERTEX_POINT('',#10442);
#2647=VERTEX_POINT('',#10444);
#2648=VERTEX_POINT('',#10448);
#2649=VERTEX_POINT('',#10450);
#2650=VERTEX_POINT('',#10454);
#2651=VERTEX_POINT('',#10456);
#2652=VERTEX_POINT('',#10460);
#2653=VERTEX_POINT('',#10462);
#2654=VERTEX_POINT('',#10472);
#2655=VERTEX_POINT('',#10473);
#2656=VERTEX_POINT('',#10475);
#2657=VERTEX_POINT('',#10477);
#2658=VERTEX_POINT('',#10481);
#2659=VERTEX_POINT('',#10483);
#2660=VERTEX_POINT('',#10487);
#2661=VERTEX_POINT('',#10489);
#2662=VERTEX_POINT('',#10493);
#2663=VERTEX_POINT('',#10495);
#2664=VERTEX_POINT('',#10499);
#2665=VERTEX_POINT('',#10501);
#2666=VERTEX_POINT('',#10510);
#2667=VERTEX_POINT('',#10513);
#2668=VERTEX_POINT('',#10516);
#2669=VERTEX_POINT('',#10520);
#2670=VERTEX_POINT('',#10524);
#2671=VERTEX_POINT('',#10528);
#2672=VERTEX_POINT('',#10531);
#2673=EDGE_CURVE('',#2262,#2262,#1995,.T.);
#2674=EDGE_CURVE('',#2262,#2263,#1351,.T.);
#2675=EDGE_CURVE('',#2263,#2263,#1996,.T.);
#2676=EDGE_CURVE('',#2264,#2264,#1997,.T.);
#2677=EDGE_CURVE('',#2264,#2265,#1352,.T.);
#2678=EDGE_CURVE('',#2265,#2265,#1998,.T.);
#2679=EDGE_CURVE('',#2266,#2266,#1999,.T.);
#2680=EDGE_CURVE('',#2266,#2267,#1353,.T.);
#2681=EDGE_CURVE('',#2267,#2267,#2000,.T.);
#2682=EDGE_CURVE('',#2268,#2268,#2001,.T.);
#2683=EDGE_CURVE('',#2268,#2269,#1354,.T.);
#2684=EDGE_CURVE('',#2269,#2269,#2002,.T.);
#2685=EDGE_CURVE('',#2270,#2271,#1355,.T.);
#2686=EDGE_CURVE('',#2271,#2272,#1356,.T.);
#2687=EDGE_CURVE('',#2273,#2272,#1357,.T.);
#2688=EDGE_CURVE('',#2270,#2273,#1358,.T.);
#2689=EDGE_CURVE('',#2274,#2270,#1359,.T.);
#2690=EDGE_CURVE('',#2275,#2273,#1360,.T.);
#2691=EDGE_CURVE('',#2274,#2275,#1361,.T.);
#2692=EDGE_CURVE('',#2276,#2274,#1362,.T.);
#2693=EDGE_CURVE('',#2277,#2275,#1363,.T.);
#2694=EDGE_CURVE('',#2276,#2277,#1364,.T.);
#2695=EDGE_CURVE('',#2271,#2276,#1365,.T.);
#2696=EDGE_CURVE('',#2272,#2277,#1366,.T.);
#2697=EDGE_CURVE('',#2278,#2279,#1367,.T.);
#2698=EDGE_CURVE('',#2279,#2280,#1368,.T.);
#2699=EDGE_CURVE('',#2281,#2280,#1369,.T.);
#2700=EDGE_CURVE('',#2278,#2281,#1370,.T.);
#2701=EDGE_CURVE('',#2282,#2278,#1371,.T.);
#2702=EDGE_CURVE('',#2283,#2281,#1372,.T.);
#2703=EDGE_CURVE('',#2282,#2283,#1373,.T.);
#2704=EDGE_CURVE('',#2284,#2282,#1374,.T.);
#2705=EDGE_CURVE('',#2285,#2283,#1375,.T.);
#2706=EDGE_CURVE('',#2284,#2285,#1376,.T.);
#2707=EDGE_CURVE('',#2279,#2284,#1377,.T.);
#2708=EDGE_CURVE('',#2280,#2285,#1378,.T.);
#2709=EDGE_CURVE('',#2286,#2287,#1379,.T.);
#2710=EDGE_CURVE('',#2287,#2288,#1380,.T.);
#2711=EDGE_CURVE('',#2289,#2288,#1381,.T.);
#2712=EDGE_CURVE('',#2286,#2289,#1382,.T.);
#2713=EDGE_CURVE('',#2290,#2286,#1383,.T.);
#2714=EDGE_CURVE('',#2291,#2289,#1384,.T.);
#2715=EDGE_CURVE('',#2290,#2291,#1385,.T.);
#2716=EDGE_CURVE('',#2292,#2290,#1386,.T.);
#2717=EDGE_CURVE('',#2293,#2291,#1387,.T.);
#2718=EDGE_CURVE('',#2292,#2293,#1388,.T.);
#2719=EDGE_CURVE('',#2287,#2292,#1389,.T.);
#2720=EDGE_CURVE('',#2288,#2293,#1390,.T.);
#2721=EDGE_CURVE('',#2294,#2295,#2003,.T.);
#2722=EDGE_CURVE('',#2294,#2295,#2004,.T.);
#2723=EDGE_CURVE('',#2296,#2296,#2005,.T.);
#2724=EDGE_CURVE('',#2297,#2294,#1391,.T.);
#2725=EDGE_CURVE('',#2298,#2297,#2006,.T.);
#2726=EDGE_CURVE('',#2295,#2298,#1392,.T.);
#2727=EDGE_CURVE('',#2299,#2300,#2007,.T.);
#2728=EDGE_CURVE('',#2299,#2300,#2008,.T.);
#2729=EDGE_CURVE('',#2301,#2301,#2009,.T.);
#2730=EDGE_CURVE('',#2302,#2299,#1393,.T.);
#2731=EDGE_CURVE('',#2303,#2302,#2010,.T.);
#2732=EDGE_CURVE('',#2300,#2303,#1394,.T.);
#2733=EDGE_CURVE('',#2304,#2305,#2011,.T.);
#2734=EDGE_CURVE('',#2304,#2305,#2012,.T.);
#2735=EDGE_CURVE('',#2306,#2306,#2013,.T.);
#2736=EDGE_CURVE('',#2307,#2304,#1395,.T.);
#2737=EDGE_CURVE('',#2308,#2307,#2014,.T.);
#2738=EDGE_CURVE('',#2305,#2308,#1396,.T.);
#2739=EDGE_CURVE('',#2309,#2310,#2015,.T.);
#2740=EDGE_CURVE('',#2309,#2310,#2016,.T.);
#2741=EDGE_CURVE('',#2311,#2311,#2017,.T.);
#2742=EDGE_CURVE('',#2312,#2309,#1397,.T.);
#2743=EDGE_CURVE('',#2313,#2312,#2018,.T.);
#2744=EDGE_CURVE('',#2310,#2313,#1398,.T.);
#2745=EDGE_CURVE('',#2297,#2313,#2019,.T.);
#2746=EDGE_CURVE('',#2312,#2308,#2020,.T.);
#2747=EDGE_CURVE('',#2307,#2303,#2021,.T.);
#2748=EDGE_CURVE('',#2302,#2314,#2022,.T.);
#2749=EDGE_CURVE('',#2314,#2298,#2023,.T.);
#2750=EDGE_CURVE('',#2315,#2315,#2024,.T.);
#2751=EDGE_CURVE('',#2314,#2316,#1399,.T.);
#2752=EDGE_CURVE('',#2316,#2316,#2025,.T.);
#2753=EDGE_CURVE('',#2317,#2317,#2026,.T.);
#2754=EDGE_CURVE('',#2317,#2318,#1400,.T.);
#2755=EDGE_CURVE('',#2318,#2318,#2027,.T.);
#2756=EDGE_CURVE('',#2319,#2320,#1401,.T.);
#2757=EDGE_CURVE('',#2321,#2319,#1402,.T.);
#2758=EDGE_CURVE('',#2321,#2322,#1403,.T.);
#2759=EDGE_CURVE('',#2322,#2323,#1404,.T.);
#2760=EDGE_CURVE('',#2323,#2324,#1405,.T.);
#2761=EDGE_CURVE('',#2324,#2320,#1406,.T.);
#2762=EDGE_CURVE('',#2325,#2321,#1407,.T.);
#2763=EDGE_CURVE('',#2326,#2325,#1408,.T.);
#2764=EDGE_CURVE('',#2326,#2322,#1409,.T.);
#2765=EDGE_CURVE('',#2327,#2328,#1410,.T.);
#2766=EDGE_CURVE('',#2327,#2324,#1411,.T.);
#2767=EDGE_CURVE('',#2328,#2323,#1412,.T.);
#2768=EDGE_CURVE('',#2328,#2326,#1413,.T.);
#2769=EDGE_CURVE('',#2329,#2320,#1414,.T.);
#2770=EDGE_CURVE('',#2330,#2329,#1415,.T.);
#2771=EDGE_CURVE('',#2330,#2319,#1416,.T.);
#2772=EDGE_CURVE('',#2331,#2327,#1417,.T.);
#2773=EDGE_CURVE('',#2331,#2332,#1418,.T.);
#2774=EDGE_CURVE('',#2332,#2333,#1419,.T.);
#2775=EDGE_CURVE('',#2333,#2334,#2028,.T.);
#2776=EDGE_CURVE('',#2334,#2329,#1420,.T.);
#2777=EDGE_CURVE('',#2335,#2334,#1421,.T.);
#2778=EDGE_CURVE('',#2335,#2330,#1422,.T.);
#2779=EDGE_CURVE('',#2333,#2336,#1423,.T.);
#2780=EDGE_CURVE('',#2337,#2332,#1424,.T.);
#2781=EDGE_CURVE('',#2337,#2336,#1425,.T.);
#2782=EDGE_CURVE('',#2338,#2337,#1426,.T.);
#2783=EDGE_CURVE('',#2338,#2331,#1427,.T.);
#2784=EDGE_CURVE('',#2325,#2338,#1428,.T.);
#2785=EDGE_CURVE('',#2336,#2335,#2029,.T.);
#2786=EDGE_CURVE('',#2335,#2339,#1429,.T.);
#2787=EDGE_CURVE('',#2339,#2339,#2030,.T.);
#2788=EDGE_CURVE('',#2340,#2341,#1430,.T.);
#2789=EDGE_CURVE('',#2341,#2342,#2031,.T.);
#2790=EDGE_CURVE('',#2342,#2343,#1431,.T.);
#2791=EDGE_CURVE('',#2343,#2340,#2032,.T.);
#2792=EDGE_CURVE('',#2344,#2345,#1432,.T.);
#2793=EDGE_CURVE('',#2345,#2346,#2033,.T.);
#2794=EDGE_CURVE('',#2346,#2347,#1433,.T.);
#2795=EDGE_CURVE('',#2347,#2344,#2034,.T.);
#2796=EDGE_CURVE('',#2348,#2348,#2035,.T.);
#2797=EDGE_CURVE('',#2348,#2349,#1434,.T.);
#2798=EDGE_CURVE('',#2349,#2349,#2036,.T.);
#2799=EDGE_CURVE('',#2350,#2351,#1435,.T.);
#2800=EDGE_CURVE('',#2352,#2350,#1436,.T.);
#2801=EDGE_CURVE('',#2352,#2353,#1437,.T.);
#2802=EDGE_CURVE('',#2351,#2353,#1438,.T.);
#2803=EDGE_CURVE('',#2354,#2355,#1439,.T.);
#2804=EDGE_CURVE('',#2356,#2354,#1440,.T.);
#2805=EDGE_CURVE('',#2357,#2356,#1441,.T.);
#2806=EDGE_CURVE('',#2355,#2357,#1442,.T.);
#2807=EDGE_CURVE('',#2357,#2358,#1443,.T.);
#2808=EDGE_CURVE('',#2359,#2356,#1444,.T.);
#2809=EDGE_CURVE('',#2358,#2359,#1445,.T.);
#2810=EDGE_CURVE('',#2358,#2352,#1446,.T.);
#2811=EDGE_CURVE('',#2353,#2359,#1447,.T.);
#2812=EDGE_CURVE('',#2355,#2360,#1448,.T.);
#2813=EDGE_CURVE('',#2360,#2350,#1449,.T.);
#2814=EDGE_CURVE('',#2361,#2360,#1450,.T.);
#2815=EDGE_CURVE('',#2346,#2361,#1451,.T.);
#2816=EDGE_CURVE('',#2345,#2362,#1452,.T.);
#2817=EDGE_CURVE('',#2354,#2362,#1453,.T.);
#2818=EDGE_CURVE('',#2363,#2351,#1454,.T.);
#2819=EDGE_CURVE('',#2364,#2363,#1455,.T.);
#2820=EDGE_CURVE('',#2361,#2364,#1456,.T.);
#2821=EDGE_CURVE('',#2344,#2365,#1457,.T.);
#2822=EDGE_CURVE('',#2362,#2365,#1458,.T.);
#2823=EDGE_CURVE('',#2364,#2347,#1459,.T.);
#2824=EDGE_CURVE('',#2365,#2363,#1460,.T.);
#2825=EDGE_CURVE('',#2366,#2366,#2037,.T.);
#2826=EDGE_CURVE('',#2366,#2367,#1461,.T.);
#2827=EDGE_CURVE('',#2367,#2367,#2038,.T.);
#2828=EDGE_CURVE('',#2368,#2369,#1462,.T.);
#2829=EDGE_CURVE('',#2370,#2368,#1463,.T.);
#2830=EDGE_CURVE('',#2370,#2371,#1464,.T.);
#2831=EDGE_CURVE('',#2371,#2372,#1465,.T.);
#2832=EDGE_CURVE('',#2372,#2373,#1466,.T.);
#2833=EDGE_CURVE('',#2373,#2369,#1467,.T.);
#2834=EDGE_CURVE('',#2374,#2370,#1468,.T.);
#2835=EDGE_CURVE('',#2375,#2374,#1469,.T.);
#2836=EDGE_CURVE('',#2375,#2371,#1470,.T.);
#2837=EDGE_CURVE('',#2369,#2376,#1471,.T.);
#2838=EDGE_CURVE('',#2377,#2373,#1472,.T.);
#2839=EDGE_CURVE('',#2376,#2377,#1473,.T.);
#2840=EDGE_CURVE('',#2377,#2378,#1474,.T.);
#2841=EDGE_CURVE('',#2378,#2372,#1475,.T.);
#2842=EDGE_CURVE('',#2378,#2375,#1476,.T.);
#2843=EDGE_CURVE('',#2374,#2379,#1477,.T.);
#2844=EDGE_CURVE('',#2379,#2380,#1478,.T.);
#2845=EDGE_CURVE('',#2380,#2381,#1479,.T.);
#2846=EDGE_CURVE('',#2381,#2376,#1480,.T.);
#2847=EDGE_CURVE('',#2380,#2341,#1481,.T.);
#2848=EDGE_CURVE('',#2379,#2382,#1482,.T.);
#2849=EDGE_CURVE('',#2342,#2382,#1483,.T.);
#2850=EDGE_CURVE('',#2381,#2340,#1484,.T.);
#2851=EDGE_CURVE('',#2383,#2343,#1485,.T.);
#2852=EDGE_CURVE('',#2368,#2383,#1486,.T.);
#2853=EDGE_CURVE('',#2382,#2383,#1487,.T.);
#2854=EDGE_CURVE('',#2384,#2384,#2039,.T.);
#2855=EDGE_CURVE('',#2384,#2296,#1488,.T.);
#2856=EDGE_CURVE('',#2385,#2385,#2040,.T.);
#2857=EDGE_CURVE('',#2385,#2301,#1489,.T.);
#2858=EDGE_CURVE('',#2386,#2386,#2041,.T.);
#2859=EDGE_CURVE('',#2386,#2306,#1490,.T.);
#2860=EDGE_CURVE('',#2387,#2387,#2042,.T.);
#2861=EDGE_CURVE('',#2387,#2311,#1491,.T.);
#2862=EDGE_CURVE('',#2388,#2388,#2043,.T.);
#2863=EDGE_CURVE('',#2389,#2389,#2044,.T.);
#2864=EDGE_CURVE('',#2390,#2390,#2045,.T.);
#2865=EDGE_CURVE('',#2390,#2388,#1492,.T.);
#2866=EDGE_CURVE('',#2389,#2315,#1493,.T.);
#2867=EDGE_CURVE('',#2391,#2392,#1494,.T.);
#2868=EDGE_CURVE('',#2392,#2393,#1495,.T.);
#2869=EDGE_CURVE('',#2394,#2393,#1496,.T.);
#2870=EDGE_CURVE('',#2391,#2394,#1497,.T.);
#2871=EDGE_CURVE('',#2395,#2391,#1498,.T.);
#2872=EDGE_CURVE('',#2396,#2394,#1499,.T.);
#2873=EDGE_CURVE('',#2395,#2396,#1500,.T.);
#2874=EDGE_CURVE('',#2397,#2395,#1501,.T.);
#2875=EDGE_CURVE('',#2398,#2396,#1502,.T.);
#2876=EDGE_CURVE('',#2397,#2398,#1503,.T.);
#2877=EDGE_CURVE('',#2392,#2397,#1504,.T.);
#2878=EDGE_CURVE('',#2393,#2398,#1505,.T.);
#2879=EDGE_CURVE('',#2399,#2399,#2046,.T.);
#2880=EDGE_CURVE('',#2399,#2400,#221,.T.);
#2881=EDGE_CURVE('',#2400,#2400,#2047,.T.);
#2882=EDGE_CURVE('',#2401,#2402,#1506,.T.);
#2883=EDGE_CURVE('',#2402,#2403,#1507,.T.);
#2884=EDGE_CURVE('',#2403,#2404,#1508,.T.);
#2885=EDGE_CURVE('',#2401,#2404,#1509,.T.);
#2886=EDGE_CURVE('',#2402,#2405,#1510,.T.);
#2887=EDGE_CURVE('',#2405,#2406,#1511,.T.);
#2888=EDGE_CURVE('',#2406,#2403,#1512,.T.);
#2889=EDGE_CURVE('',#2405,#2407,#1513,.T.);
#2890=EDGE_CURVE('',#2407,#2408,#1514,.T.);
#2891=EDGE_CURVE('',#2408,#2406,#1515,.T.);
#2892=EDGE_CURVE('',#2407,#2409,#1516,.T.);
#2893=EDGE_CURVE('',#2409,#2410,#1517,.T.);
#2894=EDGE_CURVE('',#2410,#2408,#1518,.T.);
#2895=EDGE_CURVE('',#2409,#2411,#1519,.T.);
#2896=EDGE_CURVE('',#2411,#2412,#1520,.T.);
#2897=EDGE_CURVE('',#2412,#2410,#1521,.T.);
#2898=EDGE_CURVE('',#2411,#2401,#1522,.T.);
#2899=EDGE_CURVE('',#2404,#2412,#1523,.T.);
#2900=EDGE_CURVE('',#2413,#2413,#2048,.T.);
#2901=EDGE_CURVE('',#2414,#2414,#2049,.T.);
#2902=EDGE_CURVE('',#2415,#2415,#2050,.T.);
#2903=EDGE_CURVE('',#2415,#2414,#1524,.T.);
#2904=EDGE_CURVE('',#2416,#2416,#2051,.T.);
#2905=EDGE_CURVE('',#2416,#2415,#1525,.T.);
#2906=EDGE_CURVE('',#2417,#2417,#2052,.T.);
#2907=EDGE_CURVE('',#2417,#2416,#1526,.T.);
#2908=EDGE_CURVE('',#2418,#2418,#2053,.T.);
#2909=EDGE_CURVE('',#2419,#2419,#2054,.F.);
#2910=EDGE_CURVE('',#2419,#2418,#1527,.T.);
#2911=EDGE_CURVE('',#2413,#2419,#1528,.T.);
#2912=EDGE_CURVE('',#2420,#2420,#2055,.T.);
#2913=EDGE_CURVE('',#2420,#2421,#1529,.T.);
#2914=EDGE_CURVE('',#2421,#2421,#2056,.T.);
#2915=EDGE_CURVE('',#2422,#2422,#2057,.T.);
#2916=EDGE_CURVE('',#2422,#2423,#1530,.T.);
#2917=EDGE_CURVE('',#2423,#2423,#2058,.T.);
#2918=EDGE_CURVE('',#2424,#2424,#2059,.T.);
#2919=EDGE_CURVE('',#2424,#2425,#1531,.T.);
#2920=EDGE_CURVE('',#2425,#2425,#2060,.T.);
#2921=EDGE_CURVE('',#2426,#2426,#2061,.T.);
#2922=EDGE_CURVE('',#2426,#2427,#1532,.T.);
#2923=EDGE_CURVE('',#2427,#2427,#2062,.T.);
#2924=EDGE_CURVE('',#2428,#2428,#2063,.T.);
#2925=EDGE_CURVE('',#2428,#2429,#1533,.T.);
#2926=EDGE_CURVE('',#2429,#2429,#2064,.T.);
#2927=EDGE_CURVE('',#2430,#2430,#2065,.T.);
#2928=EDGE_CURVE('',#2430,#2431,#1534,.T.);
#2929=EDGE_CURVE('',#2431,#2431,#2066,.T.);
#2930=EDGE_CURVE('',#2432,#2432,#2067,.T.);
#2931=EDGE_CURVE('',#2432,#2433,#1535,.T.);
#2932=EDGE_CURVE('',#2433,#2433,#2068,.T.);
#2933=EDGE_CURVE('',#2434,#2434,#2069,.T.);
#2934=EDGE_CURVE('',#2434,#2435,#1536,.T.);
#2935=EDGE_CURVE('',#2435,#2435,#2070,.T.);
#2936=EDGE_CURVE('',#2436,#2436,#2071,.T.);
#2937=EDGE_CURVE('',#2436,#2437,#1537,.T.);
#2938=EDGE_CURVE('',#2437,#2437,#2072,.T.);
#2939=EDGE_CURVE('',#2438,#2439,#1538,.T.);
#2940=EDGE_CURVE('',#2440,#2438,#2073,.T.);
#2941=EDGE_CURVE('',#2441,#2440,#1539,.T.);
#2942=EDGE_CURVE('',#2441,#2439,#2074,.T.);
#2943=EDGE_CURVE('',#2442,#2441,#1540,.T.);
#2944=EDGE_CURVE('',#2443,#2442,#2075,.T.);
#2945=EDGE_CURVE('',#2439,#2443,#1541,.T.);
#2946=EDGE_CURVE('',#2444,#2440,#1542,.T.);
#2947=EDGE_CURVE('',#2442,#2444,#1543,.T.);
#2948=EDGE_CURVE('',#2445,#2443,#1544,.T.);
#2949=EDGE_CURVE('',#2438,#2445,#1545,.T.);
#2950=EDGE_CURVE('',#2444,#2445,#2076,.T.);
#2951=EDGE_CURVE('',#2446,#2446,#2077,.T.);
#2952=EDGE_CURVE('',#2446,#2447,#1546,.T.);
#2953=EDGE_CURVE('',#2447,#2447,#2078,.T.);
#2954=EDGE_CURVE('',#2448,#2448,#2079,.T.);
#2955=EDGE_CURVE('',#2448,#2449,#1547,.T.);
#2956=EDGE_CURVE('',#2449,#2449,#2080,.T.);
#2957=EDGE_CURVE('',#2450,#2450,#2081,.T.);
#2958=EDGE_CURVE('',#2450,#2451,#1548,.T.);
#2959=EDGE_CURVE('',#2451,#2451,#2082,.T.);
#2960=EDGE_CURVE('',#2452,#2452,#2083,.T.);
#2961=EDGE_CURVE('',#2452,#2453,#1549,.T.);
#2962=EDGE_CURVE('',#2453,#2453,#2084,.T.);
#2963=EDGE_CURVE('',#2454,#2454,#2085,.T.);
#2964=EDGE_CURVE('',#2454,#2455,#1550,.T.);
#2965=EDGE_CURVE('',#2455,#2455,#2086,.T.);
#2966=EDGE_CURVE('',#2456,#2456,#2087,.T.);
#2967=EDGE_CURVE('',#2456,#2457,#1551,.T.);
#2968=EDGE_CURVE('',#2457,#2457,#2088,.T.);
#2969=EDGE_CURVE('',#2458,#2458,#2089,.T.);
#2970=EDGE_CURVE('',#2458,#2459,#1552,.T.);
#2971=EDGE_CURVE('',#2459,#2459,#2090,.T.);
#2972=EDGE_CURVE('',#2460,#2460,#2091,.T.);
#2973=EDGE_CURVE('',#2461,#2461,#2092,.T.);
#2974=EDGE_CURVE('',#2461,#2462,#1553,.T.);
#2975=EDGE_CURVE('',#2462,#2462,#2093,.T.);
#2976=EDGE_CURVE('',#2463,#2463,#2094,.T.);
#2977=EDGE_CURVE('',#2464,#2464,#2095,.T.);
#2978=EDGE_CURVE('',#2464,#2465,#1554,.T.);
#2979=EDGE_CURVE('',#2465,#2465,#2096,.T.);
#2980=EDGE_CURVE('',#2466,#2466,#2097,.T.);
#2981=EDGE_CURVE('',#2467,#2467,#2098,.T.);
#2982=EDGE_CURVE('',#2467,#2468,#1555,.T.);
#2983=EDGE_CURVE('',#2468,#2468,#2099,.T.);
#2984=EDGE_CURVE('',#2469,#2469,#2100,.T.);
#2985=EDGE_CURVE('',#2460,#2470,#1556,.T.);
#2986=EDGE_CURVE('',#2470,#2470,#2101,.T.);
#2987=EDGE_CURVE('',#2463,#2471,#1557,.T.);
#2988=EDGE_CURVE('',#2471,#2471,#2102,.T.);
#2989=EDGE_CURVE('',#2466,#2472,#1558,.T.);
#2990=EDGE_CURVE('',#2472,#2472,#2103,.T.);
#2991=EDGE_CURVE('',#2469,#2473,#1559,.T.);
#2992=EDGE_CURVE('',#2473,#2473,#2104,.T.);
#2993=EDGE_CURVE('',#2474,#2474,#2105,.T.);
#2994=EDGE_CURVE('',#2474,#2475,#1560,.T.);
#2995=EDGE_CURVE('',#2475,#2475,#2106,.T.);
#2996=EDGE_CURVE('',#2476,#2476,#2107,.T.);
#2997=EDGE_CURVE('',#2476,#2477,#1561,.T.);
#2998=EDGE_CURVE('',#2477,#2477,#2108,.T.);
#2999=EDGE_CURVE('',#2478,#2478,#2109,.T.);
#3000=EDGE_CURVE('',#2478,#2479,#1562,.T.);
#3001=EDGE_CURVE('',#2479,#2479,#2110,.T.);
#3002=EDGE_CURVE('',#2480,#2480,#2111,.T.);
#3003=EDGE_CURVE('',#2480,#2481,#1563,.T.);
#3004=EDGE_CURVE('',#2481,#2481,#2112,.T.);
#3005=EDGE_CURVE('',#2482,#2482,#2113,.T.);
#3006=EDGE_CURVE('',#2483,#2483,#2114,.T.);
#3007=EDGE_CURVE('',#2483,#2484,#1564,.T.);
#3008=EDGE_CURVE('',#2484,#2484,#2115,.T.);
#3009=EDGE_CURVE('',#2485,#2485,#2116,.T.);
#3010=EDGE_CURVE('',#2486,#2486,#2117,.T.);
#3011=EDGE_CURVE('',#2486,#2487,#1565,.T.);
#3012=EDGE_CURVE('',#2487,#2487,#2118,.T.);
#3013=EDGE_CURVE('',#2488,#2488,#2119,.T.);
#3014=EDGE_CURVE('',#2489,#2489,#2120,.T.);
#3015=EDGE_CURVE('',#2489,#2490,#1566,.T.);
#3016=EDGE_CURVE('',#2490,#2490,#2121,.T.);
#3017=EDGE_CURVE('',#2491,#2491,#2122,.T.);
#3018=EDGE_CURVE('',#2492,#2492,#2123,.T.);
#3019=EDGE_CURVE('',#2492,#2482,#1567,.T.);
#3020=EDGE_CURVE('',#2493,#2493,#2124,.T.);
#3021=EDGE_CURVE('',#2493,#2485,#1568,.T.);
#3022=EDGE_CURVE('',#2494,#2494,#2125,.T.);
#3023=EDGE_CURVE('',#2494,#2488,#1569,.T.);
#3024=EDGE_CURVE('',#2495,#2495,#2126,.T.);
#3025=EDGE_CURVE('',#2495,#2491,#1570,.T.);
#3026=EDGE_CURVE('',#2496,#2497,#1571,.T.);
#3027=EDGE_CURVE('',#2498,#2496,#1572,.T.);
#3028=EDGE_CURVE('',#2499,#2498,#1573,.T.);
#3029=EDGE_CURVE('',#2499,#2497,#1574,.T.);
#3030=EDGE_CURVE('',#2500,#2501,#1575,.T.);
#3031=EDGE_CURVE('',#2500,#2502,#1576,.T.);
#3032=EDGE_CURVE('',#2502,#2503,#1577,.T.);
#3033=EDGE_CURVE('',#2501,#2503,#1578,.T.);
#3034=EDGE_CURVE('',#2502,#2499,#1579,.T.);
#3035=EDGE_CURVE('',#2503,#2498,#1580,.T.);
#3036=EDGE_CURVE('',#2504,#2504,#2127,.T.);
#3037=EDGE_CURVE('',#2504,#2505,#1581,.T.);
#3038=EDGE_CURVE('',#2505,#2505,#2128,.T.);
#3039=EDGE_CURVE('',#2506,#2506,#2129,.T.);
#3040=EDGE_CURVE('',#2507,#2507,#2130,.T.);
#3041=EDGE_CURVE('',#2507,#2506,#1582,.T.);
#3042=EDGE_CURVE('',#2497,#2500,#2131,.T.);
#3043=EDGE_CURVE('',#2496,#2501,#2132,.T.);
#3044=EDGE_CURVE('',#2508,#2508,#2133,.T.);
#3045=EDGE_CURVE('',#2508,#2509,#1583,.T.);
#3046=EDGE_CURVE('',#2509,#2509,#2134,.T.);
#3047=EDGE_CURVE('',#2510,#2510,#2135,.T.);
#3048=EDGE_CURVE('',#2510,#2511,#1584,.T.);
#3049=EDGE_CURVE('',#2511,#2511,#2136,.T.);
#3050=EDGE_CURVE('',#2512,#2512,#2137,.T.);
#3051=EDGE_CURVE('',#2512,#2513,#1585,.T.);
#3052=EDGE_CURVE('',#2513,#2513,#2138,.T.);
#3053=EDGE_CURVE('',#2514,#2515,#2139,.T.);
#3054=EDGE_CURVE('',#2515,#2514,#2140,.T.);
#3055=EDGE_CURVE('',#2515,#2516,#2141,.T.);
#3056=EDGE_CURVE('',#2517,#2516,#2142,.T.);
#3057=EDGE_CURVE('',#2516,#2517,#2143,.T.);
#3058=EDGE_CURVE('',#2517,#2518,#1586,.T.);
#3059=EDGE_CURVE('',#2518,#2518,#2144,.T.);
#3060=EDGE_CURVE('',#2519,#2519,#2145,.T.);
#3061=EDGE_CURVE('',#2519,#2520,#1587,.T.);
#3062=EDGE_CURVE('',#2520,#2520,#2146,.T.);
#3063=EDGE_CURVE('',#2520,#2521,#1588,.T.);
#3064=EDGE_CURVE('',#2521,#2521,#2147,.T.);
#3065=EDGE_CURVE('',#2522,#2522,#2148,.T.);
#3066=EDGE_CURVE('',#2522,#2514,#1589,.T.);
#3067=EDGE_CURVE('',#2523,#2523,#2149,.T.);
#3068=EDGE_CURVE('',#2523,#2519,#1590,.T.);
#3069=EDGE_CURVE('',#2524,#2525,#2150,.T.);
#3070=EDGE_CURVE('',#2525,#2524,#2151,.T.);
#3071=EDGE_CURVE('',#2525,#2526,#2152,.T.);
#3072=EDGE_CURVE('',#2527,#2526,#2153,.T.);
#3073=EDGE_CURVE('',#2526,#2527,#2154,.T.);
#3074=EDGE_CURVE('',#2528,#2528,#2155,.T.);
#3075=EDGE_CURVE('',#2528,#2527,#1591,.T.);
#3076=EDGE_CURVE('',#2529,#2529,#2156,.T.);
#3077=EDGE_CURVE('',#2530,#2530,#2157,.T.);
#3078=EDGE_CURVE('',#2531,#2531,#2158,.T.);
#3079=EDGE_CURVE('',#2531,#2529,#1592,.T.);
#3080=EDGE_CURVE('',#2532,#2532,#2159,.T.);
#3081=EDGE_CURVE('',#2532,#2531,#1593,.T.);
#3082=EDGE_CURVE('',#2533,#2533,#2160,.T.);
#3083=EDGE_CURVE('',#2533,#2532,#1594,.T.);
#3084=EDGE_CURVE('',#2524,#2530,#1595,.T.);
#3085=EDGE_CURVE('',#2534,#2535,#2161,.T.);
#3086=EDGE_CURVE('',#2536,#2537,#2162,.T.);
#3087=EDGE_CURVE('',#2538,#2539,#2163,.T.);
#3088=EDGE_CURVE('',#2540,#2541,#2164,.T.);
#3089=EDGE_CURVE('',#2542,#2543,#2165,.T.);
#3090=EDGE_CURVE('',#2544,#2545,#2166,.T.);
#3091=EDGE_CURVE('',#2546,#2547,#2167,.T.);
#3092=EDGE_CURVE('',#2548,#2549,#2168,.T.);
#3093=EDGE_CURVE('',#2550,#2551,#222,.T.);
#3094=EDGE_CURVE('',#2552,#2550,#2169,.T.);
#3095=EDGE_CURVE('',#2553,#2552,#223,.T.);
#3096=EDGE_CURVE('',#2551,#2553,#2170,.T.);
#3097=EDGE_CURVE('',#2554,#2552,#2171,.T.);
#3098=EDGE_CURVE('',#2554,#2555,#224,.T.);
#3099=EDGE_CURVE('',#2556,#2555,#2172,.T.);
#3100=EDGE_CURVE('',#2556,#2557,#225,.T.);
#3101=EDGE_CURVE('',#2558,#2557,#2173,.T.);
#3102=EDGE_CURVE('',#2558,#2559,#226,.T.);
#3103=EDGE_CURVE('',#2559,#2560,#1596,.T.);
#3104=EDGE_CURVE('',#2560,#2560,#2174,.T.);
#3105=EDGE_CURVE('',#2559,#2561,#227,.T.);
#3106=EDGE_CURVE('',#2562,#2561,#2175,.T.);
#3107=EDGE_CURVE('',#2562,#2563,#228,.T.);
#3108=EDGE_CURVE('',#2564,#2563,#2176,.T.);
#3109=EDGE_CURVE('',#2564,#2565,#229,.T.);
#3110=EDGE_CURVE('',#2566,#2565,#2177,.T.);
#3111=EDGE_CURVE('',#2566,#2567,#230,.T.);
#3112=EDGE_CURVE('',#2568,#2567,#2178,.T.);
#3113=EDGE_CURVE('',#2568,#2569,#231,.T.);
#3114=EDGE_CURVE('',#2553,#2569,#2179,.T.);
#3115=EDGE_CURVE('',#2550,#2570,#2180,.T.);
#3116=EDGE_CURVE('',#2570,#2554,#2181,.T.);
#3117=EDGE_CURVE('',#2571,#2570,#232,.T.);
#3118=EDGE_CURVE('',#2555,#2571,#2182,.T.);
#3119=EDGE_CURVE('',#2571,#2572,#2183,.T.);
#3120=EDGE_CURVE('',#2572,#2556,#2184,.T.);
#3121=EDGE_CURVE('',#2573,#2572,#233,.T.);
#3122=EDGE_CURVE('',#2557,#2573,#2185,.T.);
#3123=EDGE_CURVE('',#2573,#2574,#2186,.T.);
#3124=EDGE_CURVE('',#2574,#2558,#2187,.T.);
#3125=EDGE_CURVE('',#2575,#2576,#234,.T.);
#3126=EDGE_CURVE('',#2561,#2575,#2188,.T.);
#3127=EDGE_CURVE('',#2576,#2574,#235,.T.);
#3128=EDGE_CURVE('',#2575,#2577,#2189,.T.);
#3129=EDGE_CURVE('',#2577,#2562,#2190,.T.);
#3130=EDGE_CURVE('',#2578,#2577,#236,.T.);
#3131=EDGE_CURVE('',#2563,#2578,#2191,.T.);
#3132=EDGE_CURVE('',#2578,#2579,#2192,.T.);
#3133=EDGE_CURVE('',#2579,#2564,#2193,.T.);
#3134=EDGE_CURVE('',#2580,#2579,#237,.T.);
#3135=EDGE_CURVE('',#2565,#2580,#2194,.T.);
#3136=EDGE_CURVE('',#2580,#2581,#2195,.T.);
#3137=EDGE_CURVE('',#2581,#2566,#2196,.T.);
#3138=EDGE_CURVE('',#2582,#2581,#238,.T.);
#3139=EDGE_CURVE('',#2567,#2582,#2197,.T.);
#3140=EDGE_CURVE('',#2583,#2583,#2198,.T.);
#3141=EDGE_CURVE('',#2583,#2576,#1597,.T.);
#3142=EDGE_CURVE('',#2584,#2551,#2199,.T.);
#3143=EDGE_CURVE('',#2584,#2585,#239,.T.);
#3144=EDGE_CURVE('',#2582,#2585,#2200,.T.);
#3145=EDGE_CURVE('',#2569,#2584,#2201,.T.);
#3146=EDGE_CURVE('',#2585,#2568,#2202,.T.);
#3147=EDGE_CURVE('',#2586,#2586,#2203,.T.);
#3148=EDGE_CURVE('',#2587,#2587,#2204,.T.);
#3149=EDGE_CURVE('',#2588,#2588,#2205,.T.);
#3150=EDGE_CURVE('',#2588,#2586,#1598,.T.);
#3151=EDGE_CURVE('',#2589,#2589,#2206,.T.);
#3152=EDGE_CURVE('',#2589,#2587,#1599,.T.);
#3153=EDGE_CURVE('',#2590,#2590,#2207,.T.);
#3154=EDGE_CURVE('',#2591,#2591,#2208,.T.);
#3155=EDGE_CURVE('',#2592,#2592,#2209,.T.);
#3156=EDGE_CURVE('',#2592,#2590,#1600,.T.);
#3157=EDGE_CURVE('',#2593,#2593,#2210,.T.);
#3158=EDGE_CURVE('',#2593,#2591,#1601,.T.);
#3159=EDGE_CURVE('',#2594,#2594,#2211,.T.);
#3160=EDGE_CURVE('',#2594,#2595,#1602,.T.);
#3161=EDGE_CURVE('',#2595,#2595,#2212,.T.);
#3162=EDGE_CURVE('',#2596,#2596,#2213,.T.);
#3163=EDGE_CURVE('',#2596,#2597,#1603,.T.);
#3164=EDGE_CURVE('',#2597,#2597,#2214,.T.);
#3165=EDGE_CURVE('',#2598,#2598,#2215,.T.);
#3166=EDGE_CURVE('',#2599,#2599,#2216,.T.);
#3167=EDGE_CURVE('',#2598,#2600,#1604,.T.);
#3168=EDGE_CURVE('',#2600,#2600,#2217,.T.);
#3169=EDGE_CURVE('',#2601,#2601,#2218,.T.);
#3170=EDGE_CURVE('',#2602,#2602,#2219,.T.);
#3171=EDGE_CURVE('',#2603,#2603,#2220,.T.);
#3172=EDGE_CURVE('',#2603,#2601,#1605,.T.);
#3173=EDGE_CURVE('',#2602,#2604,#1606,.T.);
#3174=EDGE_CURVE('',#2604,#2604,#2221,.T.);
#3175=EDGE_CURVE('',#2605,#2605,#2222,.T.);
#3176=EDGE_CURVE('',#2605,#2599,#1607,.T.);
#3177=EDGE_CURVE('',#2606,#2606,#2223,.T.);
#3178=EDGE_CURVE('',#2606,#2607,#1608,.T.);
#3179=EDGE_CURVE('',#2607,#2607,#2224,.T.);
#3180=EDGE_CURVE('',#2608,#2608,#2225,.T.);
#3181=EDGE_CURVE('',#2608,#2609,#1609,.T.);
#3182=EDGE_CURVE('',#2609,#2609,#2226,.T.);
#3183=EDGE_CURVE('',#2610,#2611,#1610,.T.);
#3184=EDGE_CURVE('',#2612,#2610,#2227,.T.);
#3185=EDGE_CURVE('',#2613,#2612,#1611,.T.);
#3186=EDGE_CURVE('',#2613,#2611,#2228,.T.);
#3187=EDGE_CURVE('',#2613,#2614,#1612,.T.);
#3188=EDGE_CURVE('',#2615,#2614,#2229,.T.);
#3189=EDGE_CURVE('',#2616,#2615,#2230,.T.);
#3190=EDGE_CURVE('',#2616,#2611,#1613,.T.);
#3191=EDGE_CURVE('',#2617,#2617,#2231,.T.);
#3192=EDGE_CURVE('',#2618,#2612,#1614,.T.);
#3193=EDGE_CURVE('',#2614,#2618,#1615,.T.);
#3194=EDGE_CURVE('',#2619,#2616,#1616,.T.);
#3195=EDGE_CURVE('',#2610,#2619,#1617,.T.);
#3196=EDGE_CURVE('',#2618,#2619,#2232,.T.);
#3197=EDGE_CURVE('',#2620,#2620,#2233,.T.);
#3198=EDGE_CURVE('',#2620,#2617,#1618,.T.);
#3199=EDGE_CURVE('',#2621,#2621,#2234,.T.);
#3200=EDGE_CURVE('',#2621,#2615,#1619,.T.);
#3201=EDGE_CURVE('',#2622,#2622,#2235,.T.);
#3202=EDGE_CURVE('',#2622,#2623,#1620,.T.);
#3203=EDGE_CURVE('',#2623,#2623,#2236,.T.);
#3204=EDGE_CURVE('',#2624,#2624,#2237,.T.);
#3205=EDGE_CURVE('',#2624,#2625,#1621,.T.);
#3206=EDGE_CURVE('',#2625,#2625,#2238,.T.);
#3207=EDGE_CURVE('',#2626,#2626,#2239,.T.);
#3208=EDGE_CURVE('',#2626,#2627,#1622,.T.);
#3209=EDGE_CURVE('',#2627,#2627,#2240,.T.);
#3210=EDGE_CURVE('',#2628,#2628,#2241,.T.);
#3211=EDGE_CURVE('',#2628,#2629,#1623,.T.);
#3212=EDGE_CURVE('',#2629,#2629,#2242,.T.);
#3213=EDGE_CURVE('',#2630,#2630,#2243,.T.);
#3214=EDGE_CURVE('',#2630,#2631,#1624,.T.);
#3215=EDGE_CURVE('',#2631,#2631,#2244,.T.);
#3216=EDGE_CURVE('',#2632,#2632,#2245,.T.);
#3217=EDGE_CURVE('',#2632,#2633,#1625,.T.);
#3218=EDGE_CURVE('',#2633,#2633,#2246,.T.);
#3219=EDGE_CURVE('',#2634,#2634,#2247,.T.);
#3220=EDGE_CURVE('',#2635,#2635,#2248,.T.);
#3221=EDGE_CURVE('',#2635,#2634,#1626,.T.);
#3222=EDGE_CURVE('',#2636,#2636,#2249,.T.);
#3223=EDGE_CURVE('',#2636,#2635,#1627,.T.);
#3224=EDGE_CURVE('',#2637,#2637,#2250,.T.);
#3225=EDGE_CURVE('',#2637,#2636,#1628,.T.);
#3226=EDGE_CURVE('',#2638,#2638,#2251,.T.);
#3227=EDGE_CURVE('',#2639,#2639,#2252,.F.);
#3228=EDGE_CURVE('',#2639,#2638,#1629,.T.);
#3229=EDGE_CURVE('',#2640,#2640,#2253,.F.);
#3230=EDGE_CURVE('',#2640,#2639,#1630,.T.);
#3231=EDGE_CURVE('',#2641,#2641,#2254,.T.);
#3232=EDGE_CURVE('',#2641,#2640,#1631,.T.);
#3233=EDGE_CURVE('',#2642,#2643,#1632,.T.);
#3234=EDGE_CURVE('',#2643,#2644,#1633,.T.);
#3235=EDGE_CURVE('',#2644,#2645,#1634,.T.);
#3236=EDGE_CURVE('',#2642,#2645,#1635,.T.);
#3237=EDGE_CURVE('',#2643,#2646,#1636,.T.);
#3238=EDGE_CURVE('',#2646,#2647,#1637,.T.);
#3239=EDGE_CURVE('',#2647,#2644,#1638,.T.);
#3240=EDGE_CURVE('',#2646,#2648,#1639,.T.);
#3241=EDGE_CURVE('',#2648,#2649,#1640,.T.);
#3242=EDGE_CURVE('',#2649,#2647,#1641,.T.);
#3243=EDGE_CURVE('',#2648,#2650,#1642,.T.);
#3244=EDGE_CURVE('',#2650,#2651,#1643,.T.);
#3245=EDGE_CURVE('',#2651,#2649,#1644,.T.);
#3246=EDGE_CURVE('',#2650,#2652,#1645,.T.);
#3247=EDGE_CURVE('',#2652,#2653,#1646,.T.);
#3248=EDGE_CURVE('',#2653,#2651,#1647,.T.);
#3249=EDGE_CURVE('',#2652,#2642,#1648,.T.);
#3250=EDGE_CURVE('',#2645,#2653,#1649,.T.);
#3251=EDGE_CURVE('',#2654,#2655,#1650,.T.);
#3252=EDGE_CURVE('',#2655,#2656,#1651,.T.);
#3253=EDGE_CURVE('',#2656,#2657,#1652,.T.);
#3254=EDGE_CURVE('',#2654,#2657,#1653,.T.);
#3255=EDGE_CURVE('',#2655,#2658,#1654,.T.);
#3256=EDGE_CURVE('',#2658,#2659,#1655,.T.);
#3257=EDGE_CURVE('',#2659,#2656,#1656,.T.);
#3258=EDGE_CURVE('',#2658,#2660,#1657,.T.);
#3259=EDGE_CURVE('',#2660,#2661,#1658,.T.);
#3260=EDGE_CURVE('',#2661,#2659,#1659,.T.);
#3261=EDGE_CURVE('',#2660,#2662,#1660,.T.);
#3262=EDGE_CURVE('',#2662,#2663,#1661,.T.);
#3263=EDGE_CURVE('',#2663,#2661,#1662,.T.);
#3264=EDGE_CURVE('',#2662,#2664,#1663,.T.);
#3265=EDGE_CURVE('',#2664,#2665,#1664,.T.);
#3266=EDGE_CURVE('',#2665,#2663,#1665,.T.);
#3267=EDGE_CURVE('',#2664,#2654,#1666,.T.);
#3268=EDGE_CURVE('',#2657,#2665,#1667,.T.);
#3269=EDGE_CURVE('',#2666,#2666,#2255,.T.);
#3270=EDGE_CURVE('',#2667,#2667,#2256,.T.);
#3271=EDGE_CURVE('',#2668,#2668,#2257,.T.);
#3272=EDGE_CURVE('',#2668,#2667,#1668,.T.);
#3273=EDGE_CURVE('',#2669,#2669,#2258,.T.);
#3274=EDGE_CURVE('',#2669,#2668,#1669,.T.);
#3275=EDGE_CURVE('',#2670,#2670,#2259,.T.);
#3276=EDGE_CURVE('',#2670,#2669,#1670,.T.);
#3277=EDGE_CURVE('',#2671,#2671,#2260,.T.);
#3278=EDGE_CURVE('',#2672,#2672,#2261,.F.);
#3279=EDGE_CURVE('',#2672,#2671,#1671,.T.);
#3280=EDGE_CURVE('',#2666,#2672,#1672,.T.);
#3281=ORIENTED_EDGE('',*,*,#2673,.F.);
#3282=ORIENTED_EDGE('',*,*,#2674,.T.);
#3283=ORIENTED_EDGE('',*,*,#2675,.F.);
#3284=ORIENTED_EDGE('',*,*,#2674,.F.);
#3285=ORIENTED_EDGE('',*,*,#2676,.F.);
#3286=ORIENTED_EDGE('',*,*,#2677,.T.);
#3287=ORIENTED_EDGE('',*,*,#2678,.F.);
#3288=ORIENTED_EDGE('',*,*,#2677,.F.);
#3289=ORIENTED_EDGE('',*,*,#2679,.F.);
#3290=ORIENTED_EDGE('',*,*,#2680,.T.);
#3291=ORIENTED_EDGE('',*,*,#2681,.F.);
#3292=ORIENTED_EDGE('',*,*,#2680,.F.);
#3293=ORIENTED_EDGE('',*,*,#2682,.F.);
#3294=ORIENTED_EDGE('',*,*,#2683,.T.);
#3295=ORIENTED_EDGE('',*,*,#2684,.F.);
#3296=ORIENTED_EDGE('',*,*,#2683,.F.);
#3297=ORIENTED_EDGE('',*,*,#2685,.T.);
#3298=ORIENTED_EDGE('',*,*,#2686,.T.);
#3299=ORIENTED_EDGE('',*,*,#2687,.F.);
#3300=ORIENTED_EDGE('',*,*,#2688,.F.);
#3301=ORIENTED_EDGE('',*,*,#2689,.T.);
#3302=ORIENTED_EDGE('',*,*,#2688,.T.);
#3303=ORIENTED_EDGE('',*,*,#2690,.F.);
#3304=ORIENTED_EDGE('',*,*,#2691,.F.);
#3305=ORIENTED_EDGE('',*,*,#2692,.T.);
#3306=ORIENTED_EDGE('',*,*,#2691,.T.);
#3307=ORIENTED_EDGE('',*,*,#2693,.F.);
#3308=ORIENTED_EDGE('',*,*,#2694,.F.);
#3309=ORIENTED_EDGE('',*,*,#2695,.T.);
#3310=ORIENTED_EDGE('',*,*,#2694,.T.);
#3311=ORIENTED_EDGE('',*,*,#2696,.F.);
#3312=ORIENTED_EDGE('',*,*,#2686,.F.);
#3313=ORIENTED_EDGE('',*,*,#2696,.T.);
#3314=ORIENTED_EDGE('',*,*,#2693,.T.);
#3315=ORIENTED_EDGE('',*,*,#2690,.T.);
#3316=ORIENTED_EDGE('',*,*,#2687,.T.);
#3317=ORIENTED_EDGE('',*,*,#2675,.T.);
#3318=ORIENTED_EDGE('',*,*,#2678,.T.);
#3319=ORIENTED_EDGE('',*,*,#2681,.T.);
#3320=ORIENTED_EDGE('',*,*,#2684,.T.);
#3321=ORIENTED_EDGE('',*,*,#2695,.F.);
#3322=ORIENTED_EDGE('',*,*,#2685,.F.);
#3323=ORIENTED_EDGE('',*,*,#2689,.F.);
#3324=ORIENTED_EDGE('',*,*,#2692,.F.);
#3325=ORIENTED_EDGE('',*,*,#2673,.T.);
#3326=ORIENTED_EDGE('',*,*,#2676,.T.);
#3327=ORIENTED_EDGE('',*,*,#2679,.T.);
#3328=ORIENTED_EDGE('',*,*,#2682,.T.);
#3329=ORIENTED_EDGE('',*,*,#2697,.T.);
#3330=ORIENTED_EDGE('',*,*,#2698,.T.);
#3331=ORIENTED_EDGE('',*,*,#2699,.F.);
#3332=ORIENTED_EDGE('',*,*,#2700,.F.);
#3333=ORIENTED_EDGE('',*,*,#2701,.T.);
#3334=ORIENTED_EDGE('',*,*,#2700,.T.);
#3335=ORIENTED_EDGE('',*,*,#2702,.F.);
#3336=ORIENTED_EDGE('',*,*,#2703,.F.);
#3337=ORIENTED_EDGE('',*,*,#2704,.T.);
#3338=ORIENTED_EDGE('',*,*,#2703,.T.);
#3339=ORIENTED_EDGE('',*,*,#2705,.F.);
#3340=ORIENTED_EDGE('',*,*,#2706,.F.);
#3341=ORIENTED_EDGE('',*,*,#2707,.T.);
#3342=ORIENTED_EDGE('',*,*,#2706,.T.);
#3343=ORIENTED_EDGE('',*,*,#2708,.F.);
#3344=ORIENTED_EDGE('',*,*,#2698,.F.);
#3345=ORIENTED_EDGE('',*,*,#2708,.T.);
#3346=ORIENTED_EDGE('',*,*,#2705,.T.);
#3347=ORIENTED_EDGE('',*,*,#2702,.T.);
#3348=ORIENTED_EDGE('',*,*,#2699,.T.);
#3349=ORIENTED_EDGE('',*,*,#2707,.F.);
#3350=ORIENTED_EDGE('',*,*,#2697,.F.);
#3351=ORIENTED_EDGE('',*,*,#2701,.F.);
#3352=ORIENTED_EDGE('',*,*,#2704,.F.);
#3353=ORIENTED_EDGE('',*,*,#2709,.T.);
#3354=ORIENTED_EDGE('',*,*,#2710,.T.);
#3355=ORIENTED_EDGE('',*,*,#2711,.F.);
#3356=ORIENTED_EDGE('',*,*,#2712,.F.);
#3357=ORIENTED_EDGE('',*,*,#2713,.T.);
#3358=ORIENTED_EDGE('',*,*,#2712,.T.);
#3359=ORIENTED_EDGE('',*,*,#2714,.F.);
#3360=ORIENTED_EDGE('',*,*,#2715,.F.);
#3361=ORIENTED_EDGE('',*,*,#2716,.T.);
#3362=ORIENTED_EDGE('',*,*,#2715,.T.);
#3363=ORIENTED_EDGE('',*,*,#2717,.F.);
#3364=ORIENTED_EDGE('',*,*,#2718,.F.);
#3365=ORIENTED_EDGE('',*,*,#2719,.T.);
#3366=ORIENTED_EDGE('',*,*,#2718,.T.);
#3367=ORIENTED_EDGE('',*,*,#2720,.F.);
#3368=ORIENTED_EDGE('',*,*,#2710,.F.);
#3369=ORIENTED_EDGE('',*,*,#2720,.T.);
#3370=ORIENTED_EDGE('',*,*,#2717,.T.);
#3371=ORIENTED_EDGE('',*,*,#2714,.T.);
#3372=ORIENTED_EDGE('',*,*,#2711,.T.);
#3373=ORIENTED_EDGE('',*,*,#2719,.F.);
#3374=ORIENTED_EDGE('',*,*,#2709,.F.);
#3375=ORIENTED_EDGE('',*,*,#2713,.F.);
#3376=ORIENTED_EDGE('',*,*,#2716,.F.);
#3377=ORIENTED_EDGE('',*,*,#2721,.F.);
#3378=ORIENTED_EDGE('',*,*,#2722,.T.);
#3379=ORIENTED_EDGE('',*,*,#2723,.F.);
#3380=ORIENTED_EDGE('',*,*,#2724,.F.);
#3381=ORIENTED_EDGE('',*,*,#2725,.F.);
#3382=ORIENTED_EDGE('',*,*,#2726,.F.);
#3383=ORIENTED_EDGE('',*,*,#2722,.F.);
#3384=ORIENTED_EDGE('',*,*,#2727,.F.);
#3385=ORIENTED_EDGE('',*,*,#2728,.T.);
#3386=ORIENTED_EDGE('',*,*,#2729,.F.);
#3387=ORIENTED_EDGE('',*,*,#2730,.F.);
#3388=ORIENTED_EDGE('',*,*,#2731,.F.);
#3389=ORIENTED_EDGE('',*,*,#2732,.F.);
#3390=ORIENTED_EDGE('',*,*,#2728,.F.);
#3391=ORIENTED_EDGE('',*,*,#2733,.F.);
#3392=ORIENTED_EDGE('',*,*,#2734,.T.);
#3393=ORIENTED_EDGE('',*,*,#2735,.F.);
#3394=ORIENTED_EDGE('',*,*,#2736,.F.);
#3395=ORIENTED_EDGE('',*,*,#2737,.F.);
#3396=ORIENTED_EDGE('',*,*,#2738,.F.);
#3397=ORIENTED_EDGE('',*,*,#2734,.F.);
#3398=ORIENTED_EDGE('',*,*,#2739,.F.);
#3399=ORIENTED_EDGE('',*,*,#2740,.T.);
#3400=ORIENTED_EDGE('',*,*,#2741,.F.);
#3401=ORIENTED_EDGE('',*,*,#2742,.F.);
#3402=ORIENTED_EDGE('',*,*,#2743,.F.);
#3403=ORIENTED_EDGE('',*,*,#2744,.F.);
#3404=ORIENTED_EDGE('',*,*,#2740,.F.);
#3405=ORIENTED_EDGE('',*,*,#2725,.T.);
#3406=ORIENTED_EDGE('',*,*,#2745,.T.);
#3407=ORIENTED_EDGE('',*,*,#2743,.T.);
#3408=ORIENTED_EDGE('',*,*,#2746,.T.);
#3409=ORIENTED_EDGE('',*,*,#2737,.T.);
#3410=ORIENTED_EDGE('',*,*,#2747,.T.);
#3411=ORIENTED_EDGE('',*,*,#2731,.T.);
#3412=ORIENTED_EDGE('',*,*,#2748,.T.);
#3413=ORIENTED_EDGE('',*,*,#2749,.T.);
#3414=ORIENTED_EDGE('',*,*,#2750,.T.);
#3415=ORIENTED_EDGE('',*,*,#2724,.T.);
#3416=ORIENTED_EDGE('',*,*,#2721,.T.);
#3417=ORIENTED_EDGE('',*,*,#2726,.T.);
#3418=ORIENTED_EDGE('',*,*,#2749,.F.);
#3419=ORIENTED_EDGE('',*,*,#2751,.T.);
#3420=ORIENTED_EDGE('',*,*,#2752,.T.);
#3421=ORIENTED_EDGE('',*,*,#2751,.F.);
#3422=ORIENTED_EDGE('',*,*,#2748,.F.);
#3423=ORIENTED_EDGE('',*,*,#2730,.T.);
#3424=ORIENTED_EDGE('',*,*,#2727,.T.);
#3425=ORIENTED_EDGE('',*,*,#2732,.T.);
#3426=ORIENTED_EDGE('',*,*,#2747,.F.);
#3427=ORIENTED_EDGE('',*,*,#2736,.T.);
#3428=ORIENTED_EDGE('',*,*,#2733,.T.);
#3429=ORIENTED_EDGE('',*,*,#2738,.T.);
#3430=ORIENTED_EDGE('',*,*,#2746,.F.);
#3431=ORIENTED_EDGE('',*,*,#2742,.T.);
#3432=ORIENTED_EDGE('',*,*,#2739,.T.);
#3433=ORIENTED_EDGE('',*,*,#2744,.T.);
#3434=ORIENTED_EDGE('',*,*,#2745,.F.);
#3435=ORIENTED_EDGE('',*,*,#2753,.F.);
#3436=ORIENTED_EDGE('',*,*,#2754,.T.);
#3437=ORIENTED_EDGE('',*,*,#2755,.F.);
#3438=ORIENTED_EDGE('',*,*,#2754,.F.);
#3439=ORIENTED_EDGE('',*,*,#2753,.T.);
#3440=ORIENTED_EDGE('',*,*,#2756,.F.);
#3441=ORIENTED_EDGE('',*,*,#2757,.F.);
#3442=ORIENTED_EDGE('',*,*,#2758,.T.);
#3443=ORIENTED_EDGE('',*,*,#2759,.T.);
#3444=ORIENTED_EDGE('',*,*,#2760,.T.);
#3445=ORIENTED_EDGE('',*,*,#2761,.T.);
#3446=ORIENTED_EDGE('',*,*,#2755,.T.);
#3447=ORIENTED_EDGE('',*,*,#2762,.F.);
#3448=ORIENTED_EDGE('',*,*,#2763,.F.);
#3449=ORIENTED_EDGE('',*,*,#2764,.T.);
#3450=ORIENTED_EDGE('',*,*,#2758,.F.);
#3451=ORIENTED_EDGE('',*,*,#2765,.F.);
#3452=ORIENTED_EDGE('',*,*,#2766,.T.);
#3453=ORIENTED_EDGE('',*,*,#2760,.F.);
#3454=ORIENTED_EDGE('',*,*,#2767,.F.);
#3455=ORIENTED_EDGE('',*,*,#2768,.F.);
#3456=ORIENTED_EDGE('',*,*,#2767,.T.);
#3457=ORIENTED_EDGE('',*,*,#2759,.F.);
#3458=ORIENTED_EDGE('',*,*,#2764,.F.);
#3459=ORIENTED_EDGE('',*,*,#2756,.T.);
#3460=ORIENTED_EDGE('',*,*,#2769,.F.);
#3461=ORIENTED_EDGE('',*,*,#2770,.F.);
#3462=ORIENTED_EDGE('',*,*,#2771,.T.);
#3463=ORIENTED_EDGE('',*,*,#2772,.F.);
#3464=ORIENTED_EDGE('',*,*,#2773,.T.);
#3465=ORIENTED_EDGE('',*,*,#2774,.T.);
#3466=ORIENTED_EDGE('',*,*,#2775,.T.);
#3467=ORIENTED_EDGE('',*,*,#2776,.T.);
#3468=ORIENTED_EDGE('',*,*,#2769,.T.);
#3469=ORIENTED_EDGE('',*,*,#2761,.F.);
#3470=ORIENTED_EDGE('',*,*,#2766,.F.);
#3471=ORIENTED_EDGE('',*,*,#2777,.F.);
#3472=ORIENTED_EDGE('',*,*,#2778,.T.);
#3473=ORIENTED_EDGE('',*,*,#2770,.T.);
#3474=ORIENTED_EDGE('',*,*,#2776,.F.);
#3475=ORIENTED_EDGE('',*,*,#2779,.F.);
#3476=ORIENTED_EDGE('',*,*,#2774,.F.);
#3477=ORIENTED_EDGE('',*,*,#2780,.F.);
#3478=ORIENTED_EDGE('',*,*,#2781,.T.);
#3479=ORIENTED_EDGE('',*,*,#2782,.T.);
#3480=ORIENTED_EDGE('',*,*,#2780,.T.);
#3481=ORIENTED_EDGE('',*,*,#2773,.F.);
#3482=ORIENTED_EDGE('',*,*,#2783,.F.);
#3483=ORIENTED_EDGE('',*,*,#2784,.T.);
#3484=ORIENTED_EDGE('',*,*,#2783,.T.);
#3485=ORIENTED_EDGE('',*,*,#2772,.T.);
#3486=ORIENTED_EDGE('',*,*,#2765,.T.);
#3487=ORIENTED_EDGE('',*,*,#2768,.T.);
#3488=ORIENTED_EDGE('',*,*,#2763,.T.);
#3489=ORIENTED_EDGE('',*,*,#2757,.T.);
#3490=ORIENTED_EDGE('',*,*,#2771,.F.);
#3491=ORIENTED_EDGE('',*,*,#2778,.F.);
#3492=ORIENTED_EDGE('',*,*,#2785,.F.);
#3493=ORIENTED_EDGE('',*,*,#2781,.F.);
#3494=ORIENTED_EDGE('',*,*,#2782,.F.);
#3495=ORIENTED_EDGE('',*,*,#2784,.F.);
#3496=ORIENTED_EDGE('',*,*,#2762,.T.);
#3497=ORIENTED_EDGE('',*,*,#2779,.T.);
#3498=ORIENTED_EDGE('',*,*,#2785,.T.);
#3499=ORIENTED_EDGE('',*,*,#2786,.T.);
#3500=ORIENTED_EDGE('',*,*,#2787,.F.);
#3501=ORIENTED_EDGE('',*,*,#2786,.F.);
#3502=ORIENTED_EDGE('',*,*,#2777,.T.);
#3503=ORIENTED_EDGE('',*,*,#2775,.F.);
#3504=ORIENTED_EDGE('',*,*,#2788,.T.);
#3505=ORIENTED_EDGE('',*,*,#2789,.T.);
#3506=ORIENTED_EDGE('',*,*,#2790,.T.);
#3507=ORIENTED_EDGE('',*,*,#2791,.T.);
#3508=ORIENTED_EDGE('',*,*,#2792,.T.);
#3509=ORIENTED_EDGE('',*,*,#2793,.T.);
#3510=ORIENTED_EDGE('',*,*,#2794,.T.);
#3511=ORIENTED_EDGE('',*,*,#2795,.T.);
#3512=ORIENTED_EDGE('',*,*,#2796,.F.);
#3513=ORIENTED_EDGE('',*,*,#2797,.T.);
#3514=ORIENTED_EDGE('',*,*,#2798,.F.);
#3515=ORIENTED_EDGE('',*,*,#2797,.F.);
#3516=ORIENTED_EDGE('',*,*,#2799,.F.);
#3517=ORIENTED_EDGE('',*,*,#2800,.F.);
#3518=ORIENTED_EDGE('',*,*,#2801,.T.);
#3519=ORIENTED_EDGE('',*,*,#2802,.F.);
#3520=ORIENTED_EDGE('',*,*,#2803,.F.);
#3521=ORIENTED_EDGE('',*,*,#2804,.F.);
#3522=ORIENTED_EDGE('',*,*,#2805,.F.);
#3523=ORIENTED_EDGE('',*,*,#2806,.F.);
#3524=ORIENTED_EDGE('',*,*,#2807,.F.);
#3525=ORIENTED_EDGE('',*,*,#2805,.T.);
#3526=ORIENTED_EDGE('',*,*,#2808,.F.);
#3527=ORIENTED_EDGE('',*,*,#2809,.F.);
#3528=ORIENTED_EDGE('',*,*,#2810,.F.);
#3529=ORIENTED_EDGE('',*,*,#2809,.T.);
#3530=ORIENTED_EDGE('',*,*,#2811,.F.);
#3531=ORIENTED_EDGE('',*,*,#2801,.F.);
#3532=ORIENTED_EDGE('',*,*,#2812,.F.);
#3533=ORIENTED_EDGE('',*,*,#2806,.T.);
#3534=ORIENTED_EDGE('',*,*,#2807,.T.);
#3535=ORIENTED_EDGE('',*,*,#2810,.T.);
#3536=ORIENTED_EDGE('',*,*,#2800,.T.);
#3537=ORIENTED_EDGE('',*,*,#2813,.F.);
#3538=ORIENTED_EDGE('',*,*,#2796,.T.);
#3539=ORIENTED_EDGE('',*,*,#2803,.T.);
#3540=ORIENTED_EDGE('',*,*,#2812,.T.);
#3541=ORIENTED_EDGE('',*,*,#2814,.F.);
#3542=ORIENTED_EDGE('',*,*,#2815,.F.);
#3543=ORIENTED_EDGE('',*,*,#2793,.F.);
#3544=ORIENTED_EDGE('',*,*,#2816,.T.);
#3545=ORIENTED_EDGE('',*,*,#2817,.F.);
#3546=ORIENTED_EDGE('',*,*,#2813,.T.);
#3547=ORIENTED_EDGE('',*,*,#2799,.T.);
#3548=ORIENTED_EDGE('',*,*,#2818,.F.);
#3549=ORIENTED_EDGE('',*,*,#2819,.F.);
#3550=ORIENTED_EDGE('',*,*,#2820,.F.);
#3551=ORIENTED_EDGE('',*,*,#2814,.T.);
#3552=ORIENTED_EDGE('',*,*,#2792,.F.);
#3553=ORIENTED_EDGE('',*,*,#2821,.T.);
#3554=ORIENTED_EDGE('',*,*,#2822,.F.);
#3555=ORIENTED_EDGE('',*,*,#2816,.F.);
#3556=ORIENTED_EDGE('',*,*,#2795,.F.);
#3557=ORIENTED_EDGE('',*,*,#2823,.F.);
#3558=ORIENTED_EDGE('',*,*,#2819,.T.);
#3559=ORIENTED_EDGE('',*,*,#2824,.F.);
#3560=ORIENTED_EDGE('',*,*,#2821,.F.);
#3561=ORIENTED_EDGE('',*,*,#2817,.T.);
#3562=ORIENTED_EDGE('',*,*,#2822,.T.);
#3563=ORIENTED_EDGE('',*,*,#2824,.T.);
#3564=ORIENTED_EDGE('',*,*,#2818,.T.);
#3565=ORIENTED_EDGE('',*,*,#2802,.T.);
#3566=ORIENTED_EDGE('',*,*,#2811,.T.);
#3567=ORIENTED_EDGE('',*,*,#2808,.T.);
#3568=ORIENTED_EDGE('',*,*,#2804,.T.);
#3569=ORIENTED_EDGE('',*,*,#2798,.T.);
#3570=ORIENTED_EDGE('',*,*,#2794,.F.);
#3571=ORIENTED_EDGE('',*,*,#2815,.T.);
#3572=ORIENTED_EDGE('',*,*,#2820,.T.);
#3573=ORIENTED_EDGE('',*,*,#2823,.T.);
#3574=ORIENTED_EDGE('',*,*,#2825,.F.);
#3575=ORIENTED_EDGE('',*,*,#2826,.T.);
#3576=ORIENTED_EDGE('',*,*,#2827,.F.);
#3577=ORIENTED_EDGE('',*,*,#2826,.F.);
#3578=ORIENTED_EDGE('',*,*,#2828,.F.);
#3579=ORIENTED_EDGE('',*,*,#2829,.F.);
#3580=ORIENTED_EDGE('',*,*,#2830,.T.);
#3581=ORIENTED_EDGE('',*,*,#2831,.T.);
#3582=ORIENTED_EDGE('',*,*,#2832,.T.);
#3583=ORIENTED_EDGE('',*,*,#2833,.T.);
#3584=ORIENTED_EDGE('',*,*,#2827,.T.);
#3585=ORIENTED_EDGE('',*,*,#2834,.F.);
#3586=ORIENTED_EDGE('',*,*,#2835,.F.);
#3587=ORIENTED_EDGE('',*,*,#2836,.T.);
#3588=ORIENTED_EDGE('',*,*,#2830,.F.);
#3589=ORIENTED_EDGE('',*,*,#2837,.F.);
#3590=ORIENTED_EDGE('',*,*,#2833,.F.);
#3591=ORIENTED_EDGE('',*,*,#2838,.F.);
#3592=ORIENTED_EDGE('',*,*,#2839,.F.);
#3593=ORIENTED_EDGE('',*,*,#2840,.F.);
#3594=ORIENTED_EDGE('',*,*,#2838,.T.);
#3595=ORIENTED_EDGE('',*,*,#2832,.F.);
#3596=ORIENTED_EDGE('',*,*,#2841,.F.);
#3597=ORIENTED_EDGE('',*,*,#2842,.F.);
#3598=ORIENTED_EDGE('',*,*,#2841,.T.);
#3599=ORIENTED_EDGE('',*,*,#2831,.F.);
#3600=ORIENTED_EDGE('',*,*,#2836,.F.);
#3601=ORIENTED_EDGE('',*,*,#2839,.T.);
#3602=ORIENTED_EDGE('',*,*,#2840,.T.);
#3603=ORIENTED_EDGE('',*,*,#2842,.T.);
#3604=ORIENTED_EDGE('',*,*,#2835,.T.);
#3605=ORIENTED_EDGE('',*,*,#2843,.T.);
#3606=ORIENTED_EDGE('',*,*,#2844,.T.);
#3607=ORIENTED_EDGE('',*,*,#2845,.T.);
#3608=ORIENTED_EDGE('',*,*,#2846,.T.);
#3609=ORIENTED_EDGE('',*,*,#2825,.T.);
#3610=ORIENTED_EDGE('',*,*,#2789,.F.);
#3611=ORIENTED_EDGE('',*,*,#2847,.F.);
#3612=ORIENTED_EDGE('',*,*,#2844,.F.);
#3613=ORIENTED_EDGE('',*,*,#2848,.T.);
#3614=ORIENTED_EDGE('',*,*,#2849,.F.);
#3615=ORIENTED_EDGE('',*,*,#2788,.F.);
#3616=ORIENTED_EDGE('',*,*,#2850,.F.);
#3617=ORIENTED_EDGE('',*,*,#2845,.F.);
#3618=ORIENTED_EDGE('',*,*,#2847,.T.);
#3619=ORIENTED_EDGE('',*,*,#2837,.T.);
#3620=ORIENTED_EDGE('',*,*,#2846,.F.);
#3621=ORIENTED_EDGE('',*,*,#2850,.T.);
#3622=ORIENTED_EDGE('',*,*,#2791,.F.);
#3623=ORIENTED_EDGE('',*,*,#2851,.F.);
#3624=ORIENTED_EDGE('',*,*,#2852,.F.);
#3625=ORIENTED_EDGE('',*,*,#2828,.T.);
#3626=ORIENTED_EDGE('',*,*,#2829,.T.);
#3627=ORIENTED_EDGE('',*,*,#2852,.T.);
#3628=ORIENTED_EDGE('',*,*,#2853,.F.);
#3629=ORIENTED_EDGE('',*,*,#2848,.F.);
#3630=ORIENTED_EDGE('',*,*,#2843,.F.);
#3631=ORIENTED_EDGE('',*,*,#2834,.T.);
#3632=ORIENTED_EDGE('',*,*,#2790,.F.);
#3633=ORIENTED_EDGE('',*,*,#2849,.T.);
#3634=ORIENTED_EDGE('',*,*,#2853,.T.);
#3635=ORIENTED_EDGE('',*,*,#2851,.T.);
#3636=ORIENTED_EDGE('',*,*,#2854,.F.);
#3637=ORIENTED_EDGE('',*,*,#2855,.T.);
#3638=ORIENTED_EDGE('',*,*,#2723,.T.);
#3639=ORIENTED_EDGE('',*,*,#2855,.F.);
#3640=ORIENTED_EDGE('',*,*,#2856,.F.);
#3641=ORIENTED_EDGE('',*,*,#2857,.T.);
#3642=ORIENTED_EDGE('',*,*,#2729,.T.);
#3643=ORIENTED_EDGE('',*,*,#2857,.F.);
#3644=ORIENTED_EDGE('',*,*,#2858,.F.);
#3645=ORIENTED_EDGE('',*,*,#2859,.T.);
#3646=ORIENTED_EDGE('',*,*,#2735,.T.);
#3647=ORIENTED_EDGE('',*,*,#2859,.F.);
#3648=ORIENTED_EDGE('',*,*,#2860,.F.);
#3649=ORIENTED_EDGE('',*,*,#2861,.T.);
#3650=ORIENTED_EDGE('',*,*,#2741,.T.);
#3651=ORIENTED_EDGE('',*,*,#2861,.F.);
#3652=ORIENTED_EDGE('',*,*,#2862,.F.);
#3653=ORIENTED_EDGE('',*,*,#2863,.T.);
#3654=ORIENTED_EDGE('',*,*,#2864,.F.);
#3655=ORIENTED_EDGE('',*,*,#2865,.T.);
#3656=ORIENTED_EDGE('',*,*,#2862,.T.);
#3657=ORIENTED_EDGE('',*,*,#2865,.F.);
#3658=ORIENTED_EDGE('',*,*,#2864,.T.);
#3659=ORIENTED_EDGE('',*,*,#2787,.T.);
#3660=ORIENTED_EDGE('',*,*,#2863,.F.);
#3661=ORIENTED_EDGE('',*,*,#2866,.T.);
#3662=ORIENTED_EDGE('',*,*,#2750,.F.);
#3663=ORIENTED_EDGE('',*,*,#2866,.F.);
#3664=ORIENTED_EDGE('',*,*,#2752,.F.);
#3665=ORIENTED_EDGE('',*,*,#2854,.T.);
#3666=ORIENTED_EDGE('',*,*,#2856,.T.);
#3667=ORIENTED_EDGE('',*,*,#2858,.T.);
#3668=ORIENTED_EDGE('',*,*,#2860,.T.);
#3669=ORIENTED_EDGE('',*,*,#2867,.T.);
#3670=ORIENTED_EDGE('',*,*,#2868,.T.);
#3671=ORIENTED_EDGE('',*,*,#2869,.F.);
#3672=ORIENTED_EDGE('',*,*,#2870,.F.);
#3673=ORIENTED_EDGE('',*,*,#2871,.T.);
#3674=ORIENTED_EDGE('',*,*,#2870,.T.);
#3675=ORIENTED_EDGE('',*,*,#2872,.F.);
#3676=ORIENTED_EDGE('',*,*,#2873,.F.);
#3677=ORIENTED_EDGE('',*,*,#2874,.T.);
#3678=ORIENTED_EDGE('',*,*,#2873,.T.);
#3679=ORIENTED_EDGE('',*,*,#2875,.F.);
#3680=ORIENTED_EDGE('',*,*,#2876,.F.);
#3681=ORIENTED_EDGE('',*,*,#2877,.T.);
#3682=ORIENTED_EDGE('',*,*,#2876,.T.);
#3683=ORIENTED_EDGE('',*,*,#2878,.F.);
#3684=ORIENTED_EDGE('',*,*,#2868,.F.);
#3685=ORIENTED_EDGE('',*,*,#2878,.T.);
#3686=ORIENTED_EDGE('',*,*,#2875,.T.);
#3687=ORIENTED_EDGE('',*,*,#2872,.T.);
#3688=ORIENTED_EDGE('',*,*,#2869,.T.);
#3689=ORIENTED_EDGE('',*,*,#2877,.F.);
#3690=ORIENTED_EDGE('',*,*,#2867,.F.);
#3691=ORIENTED_EDGE('',*,*,#2871,.F.);
#3692=ORIENTED_EDGE('',*,*,#2874,.F.);
#3693=ORIENTED_EDGE('',*,*,#2879,.T.);
#3694=ORIENTED_EDGE('',*,*,#2880,.T.);
#3695=ORIENTED_EDGE('',*,*,#2881,.F.);
#3696=ORIENTED_EDGE('',*,*,#2880,.F.);
#3697=ORIENTED_EDGE('',*,*,#2881,.T.);
#3698=ORIENTED_EDGE('',*,*,#2879,.F.);
#3699=ORIENTED_EDGE('',*,*,#2882,.T.);
#3700=ORIENTED_EDGE('',*,*,#2883,.T.);
#3701=ORIENTED_EDGE('',*,*,#2884,.T.);
#3702=ORIENTED_EDGE('',*,*,#2885,.F.);
#3703=ORIENTED_EDGE('',*,*,#2886,.T.);
#3704=ORIENTED_EDGE('',*,*,#2887,.T.);
#3705=ORIENTED_EDGE('',*,*,#2888,.T.);
#3706=ORIENTED_EDGE('',*,*,#2883,.F.);
#3707=ORIENTED_EDGE('',*,*,#2889,.T.);
#3708=ORIENTED_EDGE('',*,*,#2890,.T.);
#3709=ORIENTED_EDGE('',*,*,#2891,.T.);
#3710=ORIENTED_EDGE('',*,*,#2887,.F.);
#3711=ORIENTED_EDGE('',*,*,#2892,.T.);
#3712=ORIENTED_EDGE('',*,*,#2893,.T.);
#3713=ORIENTED_EDGE('',*,*,#2894,.T.);
#3714=ORIENTED_EDGE('',*,*,#2890,.F.);
#3715=ORIENTED_EDGE('',*,*,#2895,.T.);
#3716=ORIENTED_EDGE('',*,*,#2896,.T.);
#3717=ORIENTED_EDGE('',*,*,#2897,.T.);
#3718=ORIENTED_EDGE('',*,*,#2893,.F.);
#3719=ORIENTED_EDGE('',*,*,#2898,.T.);
#3720=ORIENTED_EDGE('',*,*,#2885,.T.);
#3721=ORIENTED_EDGE('',*,*,#2899,.T.);
#3722=ORIENTED_EDGE('',*,*,#2896,.F.);
#3723=ORIENTED_EDGE('',*,*,#2898,.F.);
#3724=ORIENTED_EDGE('',*,*,#2895,.F.);
#3725=ORIENTED_EDGE('',*,*,#2892,.F.);
#3726=ORIENTED_EDGE('',*,*,#2889,.F.);
#3727=ORIENTED_EDGE('',*,*,#2886,.F.);
#3728=ORIENTED_EDGE('',*,*,#2882,.F.);
#3729=ORIENTED_EDGE('',*,*,#2899,.F.);
#3730=ORIENTED_EDGE('',*,*,#2884,.F.);
#3731=ORIENTED_EDGE('',*,*,#2888,.F.);
#3732=ORIENTED_EDGE('',*,*,#2891,.F.);
#3733=ORIENTED_EDGE('',*,*,#2894,.F.);
#3734=ORIENTED_EDGE('',*,*,#2897,.F.);
#3735=ORIENTED_EDGE('',*,*,#2900,.F.);
#3736=ORIENTED_EDGE('',*,*,#2901,.F.);
#3737=ORIENTED_EDGE('',*,*,#2902,.F.);
#3738=ORIENTED_EDGE('',*,*,#2903,.T.);
#3739=ORIENTED_EDGE('',*,*,#2901,.T.);
#3740=ORIENTED_EDGE('',*,*,#2903,.F.);
#3741=ORIENTED_EDGE('',*,*,#2904,.F.);
#3742=ORIENTED_EDGE('',*,*,#2905,.T.);
#3743=ORIENTED_EDGE('',*,*,#2902,.T.);
#3744=ORIENTED_EDGE('',*,*,#2905,.F.);
#3745=ORIENTED_EDGE('',*,*,#2906,.F.);
#3746=ORIENTED_EDGE('',*,*,#2907,.T.);
#3747=ORIENTED_EDGE('',*,*,#2904,.T.);
#3748=ORIENTED_EDGE('',*,*,#2907,.F.);
#3749=ORIENTED_EDGE('',*,*,#2906,.T.);
#3750=ORIENTED_EDGE('',*,*,#2908,.F.);
#3751=ORIENTED_EDGE('',*,*,#2909,.F.);
#3752=ORIENTED_EDGE('',*,*,#2910,.T.);
#3753=ORIENTED_EDGE('',*,*,#2908,.T.);
#3754=ORIENTED_EDGE('',*,*,#2910,.F.);
#3755=ORIENTED_EDGE('',*,*,#2900,.T.);
#3756=ORIENTED_EDGE('',*,*,#2911,.T.);
#3757=ORIENTED_EDGE('',*,*,#2909,.T.);
#3758=ORIENTED_EDGE('',*,*,#2911,.F.);
#3759=ORIENTED_EDGE('',*,*,#2912,.F.);
#3760=ORIENTED_EDGE('',*,*,#2913,.T.);
#3761=ORIENTED_EDGE('',*,*,#2914,.F.);
#3762=ORIENTED_EDGE('',*,*,#2913,.F.);
#3763=ORIENTED_EDGE('',*,*,#2912,.T.);
#3764=ORIENTED_EDGE('',*,*,#2915,.F.);
#3765=ORIENTED_EDGE('',*,*,#2916,.T.);
#3766=ORIENTED_EDGE('',*,*,#2917,.F.);
#3767=ORIENTED_EDGE('',*,*,#2916,.F.);
#3768=ORIENTED_EDGE('',*,*,#2915,.T.);
#3769=ORIENTED_EDGE('',*,*,#2918,.F.);
#3770=ORIENTED_EDGE('',*,*,#2919,.T.);
#3771=ORIENTED_EDGE('',*,*,#2920,.F.);
#3772=ORIENTED_EDGE('',*,*,#2919,.F.);
#3773=ORIENTED_EDGE('',*,*,#2918,.T.);
#3774=ORIENTED_EDGE('',*,*,#2921,.F.);
#3775=ORIENTED_EDGE('',*,*,#2922,.T.);
#3776=ORIENTED_EDGE('',*,*,#2923,.F.);
#3777=ORIENTED_EDGE('',*,*,#2922,.F.);
#3778=ORIENTED_EDGE('',*,*,#2921,.T.);
#3779=ORIENTED_EDGE('',*,*,#2924,.F.);
#3780=ORIENTED_EDGE('',*,*,#2925,.T.);
#3781=ORIENTED_EDGE('',*,*,#2926,.T.);
#3782=ORIENTED_EDGE('',*,*,#2925,.F.);
#3783=ORIENTED_EDGE('',*,*,#2926,.F.);
#3784=ORIENTED_EDGE('',*,*,#2927,.F.);
#3785=ORIENTED_EDGE('',*,*,#2928,.T.);
#3786=ORIENTED_EDGE('',*,*,#2929,.T.);
#3787=ORIENTED_EDGE('',*,*,#2928,.F.);
#3788=ORIENTED_EDGE('',*,*,#2929,.F.);
#3789=ORIENTED_EDGE('',*,*,#2930,.F.);
#3790=ORIENTED_EDGE('',*,*,#2931,.T.);
#3791=ORIENTED_EDGE('',*,*,#2932,.T.);
#3792=ORIENTED_EDGE('',*,*,#2931,.F.);
#3793=ORIENTED_EDGE('',*,*,#2932,.F.);
#3794=ORIENTED_EDGE('',*,*,#2933,.F.);
#3795=ORIENTED_EDGE('',*,*,#2934,.T.);
#3796=ORIENTED_EDGE('',*,*,#2935,.T.);
#3797=ORIENTED_EDGE('',*,*,#2934,.F.);
#3798=ORIENTED_EDGE('',*,*,#2935,.F.);
#3799=ORIENTED_EDGE('',*,*,#2936,.F.);
#3800=ORIENTED_EDGE('',*,*,#2937,.T.);
#3801=ORIENTED_EDGE('',*,*,#2938,.T.);
#3802=ORIENTED_EDGE('',*,*,#2937,.F.);
#3803=ORIENTED_EDGE('',*,*,#2938,.F.);
#3804=ORIENTED_EDGE('',*,*,#2939,.F.);
#3805=ORIENTED_EDGE('',*,*,#2940,.F.);
#3806=ORIENTED_EDGE('',*,*,#2941,.F.);
#3807=ORIENTED_EDGE('',*,*,#2942,.T.);
#3808=ORIENTED_EDGE('',*,*,#2942,.F.);
#3809=ORIENTED_EDGE('',*,*,#2943,.F.);
#3810=ORIENTED_EDGE('',*,*,#2944,.F.);
#3811=ORIENTED_EDGE('',*,*,#2945,.F.);
#3812=ORIENTED_EDGE('',*,*,#2936,.T.);
#3813=ORIENTED_EDGE('',*,*,#2941,.T.);
#3814=ORIENTED_EDGE('',*,*,#2946,.F.);
#3815=ORIENTED_EDGE('',*,*,#2947,.F.);
#3816=ORIENTED_EDGE('',*,*,#2943,.T.);
#3817=ORIENTED_EDGE('',*,*,#2939,.T.);
#3818=ORIENTED_EDGE('',*,*,#2945,.T.);
#3819=ORIENTED_EDGE('',*,*,#2948,.F.);
#3820=ORIENTED_EDGE('',*,*,#2949,.F.);
#3821=ORIENTED_EDGE('',*,*,#2949,.T.);
#3822=ORIENTED_EDGE('',*,*,#2950,.F.);
#3823=ORIENTED_EDGE('',*,*,#2946,.T.);
#3824=ORIENTED_EDGE('',*,*,#2940,.T.);
#3825=ORIENTED_EDGE('',*,*,#2951,.F.);
#3826=ORIENTED_EDGE('',*,*,#2952,.T.);
#3827=ORIENTED_EDGE('',*,*,#2953,.T.);
#3828=ORIENTED_EDGE('',*,*,#2952,.F.);
#3829=ORIENTED_EDGE('',*,*,#2954,.F.);
#3830=ORIENTED_EDGE('',*,*,#2955,.T.);
#3831=ORIENTED_EDGE('',*,*,#2956,.T.);
#3832=ORIENTED_EDGE('',*,*,#2955,.F.);
#3833=ORIENTED_EDGE('',*,*,#2947,.T.);
#3834=ORIENTED_EDGE('',*,*,#2950,.T.);
#3835=ORIENTED_EDGE('',*,*,#2948,.T.);
#3836=ORIENTED_EDGE('',*,*,#2944,.T.);
#3837=ORIENTED_EDGE('',*,*,#2954,.T.);
#3838=ORIENTED_EDGE('',*,*,#2951,.T.);
#3839=ORIENTED_EDGE('',*,*,#2923,.T.);
#3840=ORIENTED_EDGE('',*,*,#2920,.T.);
#3841=ORIENTED_EDGE('',*,*,#2917,.T.);
#3842=ORIENTED_EDGE('',*,*,#2914,.T.);
#3843=ORIENTED_EDGE('',*,*,#2956,.F.);
#3844=ORIENTED_EDGE('',*,*,#2953,.F.);
#3845=ORIENTED_EDGE('',*,*,#2933,.T.);
#3846=ORIENTED_EDGE('',*,*,#2930,.T.);
#3847=ORIENTED_EDGE('',*,*,#2927,.T.);
#3848=ORIENTED_EDGE('',*,*,#2924,.T.);
#3849=ORIENTED_EDGE('',*,*,#2957,.F.);
#3850=ORIENTED_EDGE('',*,*,#2958,.T.);
#3851=ORIENTED_EDGE('',*,*,#2959,.T.);
#3852=ORIENTED_EDGE('',*,*,#2958,.F.);
#3853=ORIENTED_EDGE('',*,*,#2960,.F.);
#3854=ORIENTED_EDGE('',*,*,#2961,.T.);
#3855=ORIENTED_EDGE('',*,*,#2962,.T.);
#3856=ORIENTED_EDGE('',*,*,#2961,.F.);
#3857=ORIENTED_EDGE('',*,*,#2960,.T.);
#3858=ORIENTED_EDGE('',*,*,#2957,.T.);
#3859=ORIENTED_EDGE('',*,*,#2962,.F.);
#3860=ORIENTED_EDGE('',*,*,#2959,.F.);
#3861=ORIENTED_EDGE('',*,*,#2963,.F.);
#3862=ORIENTED_EDGE('',*,*,#2964,.T.);
#3863=ORIENTED_EDGE('',*,*,#2965,.T.);
#3864=ORIENTED_EDGE('',*,*,#2964,.F.);
#3865=ORIENTED_EDGE('',*,*,#2966,.F.);
#3866=ORIENTED_EDGE('',*,*,#2967,.T.);
#3867=ORIENTED_EDGE('',*,*,#2968,.T.);
#3868=ORIENTED_EDGE('',*,*,#2967,.F.);
#3869=ORIENTED_EDGE('',*,*,#2966,.T.);
#3870=ORIENTED_EDGE('',*,*,#2963,.T.);
#3871=ORIENTED_EDGE('',*,*,#2968,.F.);
#3872=ORIENTED_EDGE('',*,*,#2965,.F.);
#3873=ORIENTED_EDGE('',*,*,#2969,.F.);
#3874=ORIENTED_EDGE('',*,*,#2970,.T.);
#3875=ORIENTED_EDGE('',*,*,#2971,.T.);
#3876=ORIENTED_EDGE('',*,*,#2970,.F.);
#3877=ORIENTED_EDGE('',*,*,#2971,.F.);
#3878=ORIENTED_EDGE('',*,*,#2972,.F.);
#3879=ORIENTED_EDGE('',*,*,#2973,.F.);
#3880=ORIENTED_EDGE('',*,*,#2974,.T.);
#3881=ORIENTED_EDGE('',*,*,#2975,.T.);
#3882=ORIENTED_EDGE('',*,*,#2974,.F.);
#3883=ORIENTED_EDGE('',*,*,#2975,.F.);
#3884=ORIENTED_EDGE('',*,*,#2976,.F.);
#3885=ORIENTED_EDGE('',*,*,#2977,.F.);
#3886=ORIENTED_EDGE('',*,*,#2978,.T.);
#3887=ORIENTED_EDGE('',*,*,#2979,.T.);
#3888=ORIENTED_EDGE('',*,*,#2978,.F.);
#3889=ORIENTED_EDGE('',*,*,#2979,.F.);
#3890=ORIENTED_EDGE('',*,*,#2980,.F.);
#3891=ORIENTED_EDGE('',*,*,#2981,.F.);
#3892=ORIENTED_EDGE('',*,*,#2982,.T.);
#3893=ORIENTED_EDGE('',*,*,#2983,.T.);
#3894=ORIENTED_EDGE('',*,*,#2982,.F.);
#3895=ORIENTED_EDGE('',*,*,#2983,.F.);
#3896=ORIENTED_EDGE('',*,*,#2984,.F.);
#3897=ORIENTED_EDGE('',*,*,#2972,.T.);
#3898=ORIENTED_EDGE('',*,*,#2985,.T.);
#3899=ORIENTED_EDGE('',*,*,#2986,.F.);
#3900=ORIENTED_EDGE('',*,*,#2985,.F.);
#3901=ORIENTED_EDGE('',*,*,#2976,.T.);
#3902=ORIENTED_EDGE('',*,*,#2987,.T.);
#3903=ORIENTED_EDGE('',*,*,#2988,.F.);
#3904=ORIENTED_EDGE('',*,*,#2987,.F.);
#3905=ORIENTED_EDGE('',*,*,#2980,.T.);
#3906=ORIENTED_EDGE('',*,*,#2989,.T.);
#3907=ORIENTED_EDGE('',*,*,#2990,.F.);
#3908=ORIENTED_EDGE('',*,*,#2989,.F.);
#3909=ORIENTED_EDGE('',*,*,#2984,.T.);
#3910=ORIENTED_EDGE('',*,*,#2991,.T.);
#3911=ORIENTED_EDGE('',*,*,#2992,.F.);
#3912=ORIENTED_EDGE('',*,*,#2991,.F.);
#3913=ORIENTED_EDGE('',*,*,#2993,.F.);
#3914=ORIENTED_EDGE('',*,*,#2994,.T.);
#3915=ORIENTED_EDGE('',*,*,#2995,.F.);
#3916=ORIENTED_EDGE('',*,*,#2994,.F.);
#3917=ORIENTED_EDGE('',*,*,#2993,.T.);
#3918=ORIENTED_EDGE('',*,*,#2996,.T.);
#3919=ORIENTED_EDGE('',*,*,#2996,.F.);
#3920=ORIENTED_EDGE('',*,*,#2997,.T.);
#3921=ORIENTED_EDGE('',*,*,#2998,.T.);
#3922=ORIENTED_EDGE('',*,*,#2997,.F.);
#3923=ORIENTED_EDGE('',*,*,#2999,.F.);
#3924=ORIENTED_EDGE('',*,*,#3000,.T.);
#3925=ORIENTED_EDGE('',*,*,#3001,.T.);
#3926=ORIENTED_EDGE('',*,*,#3000,.F.);
#3927=ORIENTED_EDGE('',*,*,#2999,.T.);
#3928=ORIENTED_EDGE('',*,*,#2995,.T.);
#3929=ORIENTED_EDGE('',*,*,#2992,.T.);
#3930=ORIENTED_EDGE('',*,*,#2990,.T.);
#3931=ORIENTED_EDGE('',*,*,#2988,.T.);
#3932=ORIENTED_EDGE('',*,*,#2986,.T.);
#3933=ORIENTED_EDGE('',*,*,#3001,.F.);
#3934=ORIENTED_EDGE('',*,*,#2998,.F.);
#3935=ORIENTED_EDGE('',*,*,#2981,.T.);
#3936=ORIENTED_EDGE('',*,*,#2977,.T.);
#3937=ORIENTED_EDGE('',*,*,#2973,.T.);
#3938=ORIENTED_EDGE('',*,*,#2969,.T.);
#3939=ORIENTED_EDGE('',*,*,#3002,.F.);
#3940=ORIENTED_EDGE('',*,*,#3003,.T.);
#3941=ORIENTED_EDGE('',*,*,#3004,.F.);
#3942=ORIENTED_EDGE('',*,*,#3003,.F.);
#3943=ORIENTED_EDGE('',*,*,#3002,.T.);
#3944=ORIENTED_EDGE('',*,*,#3005,.F.);
#3945=ORIENTED_EDGE('',*,*,#3006,.F.);
#3946=ORIENTED_EDGE('',*,*,#3007,.T.);
#3947=ORIENTED_EDGE('',*,*,#3008,.F.);
#3948=ORIENTED_EDGE('',*,*,#3007,.F.);
#3949=ORIENTED_EDGE('',*,*,#3006,.T.);
#3950=ORIENTED_EDGE('',*,*,#3009,.F.);
#3951=ORIENTED_EDGE('',*,*,#3010,.F.);
#3952=ORIENTED_EDGE('',*,*,#3011,.T.);
#3953=ORIENTED_EDGE('',*,*,#3012,.F.);
#3954=ORIENTED_EDGE('',*,*,#3011,.F.);
#3955=ORIENTED_EDGE('',*,*,#3010,.T.);
#3956=ORIENTED_EDGE('',*,*,#3013,.F.);
#3957=ORIENTED_EDGE('',*,*,#3014,.F.);
#3958=ORIENTED_EDGE('',*,*,#3015,.T.);
#3959=ORIENTED_EDGE('',*,*,#3016,.F.);
#3960=ORIENTED_EDGE('',*,*,#3015,.F.);
#3961=ORIENTED_EDGE('',*,*,#3014,.T.);
#3962=ORIENTED_EDGE('',*,*,#3017,.F.);
#3963=ORIENTED_EDGE('',*,*,#3018,.F.);
#3964=ORIENTED_EDGE('',*,*,#3019,.T.);
#3965=ORIENTED_EDGE('',*,*,#3005,.T.);
#3966=ORIENTED_EDGE('',*,*,#3019,.F.);
#3967=ORIENTED_EDGE('',*,*,#3020,.F.);
#3968=ORIENTED_EDGE('',*,*,#3021,.T.);
#3969=ORIENTED_EDGE('',*,*,#3009,.T.);
#3970=ORIENTED_EDGE('',*,*,#3021,.F.);
#3971=ORIENTED_EDGE('',*,*,#3022,.F.);
#3972=ORIENTED_EDGE('',*,*,#3023,.T.);
#3973=ORIENTED_EDGE('',*,*,#3013,.T.);
#3974=ORIENTED_EDGE('',*,*,#3023,.F.);
#3975=ORIENTED_EDGE('',*,*,#3024,.F.);
#3976=ORIENTED_EDGE('',*,*,#3025,.T.);
#3977=ORIENTED_EDGE('',*,*,#3017,.T.);
#3978=ORIENTED_EDGE('',*,*,#3025,.F.);
#3979=ORIENTED_EDGE('',*,*,#3026,.F.);
#3980=ORIENTED_EDGE('',*,*,#3027,.F.);
#3981=ORIENTED_EDGE('',*,*,#3028,.F.);
#3982=ORIENTED_EDGE('',*,*,#3029,.T.);
#3983=ORIENTED_EDGE('',*,*,#3030,.F.);
#3984=ORIENTED_EDGE('',*,*,#3031,.T.);
#3985=ORIENTED_EDGE('',*,*,#3032,.T.);
#3986=ORIENTED_EDGE('',*,*,#3033,.F.);
#3987=ORIENTED_EDGE('',*,*,#3034,.T.);
#3988=ORIENTED_EDGE('',*,*,#3028,.T.);
#3989=ORIENTED_EDGE('',*,*,#3035,.F.);
#3990=ORIENTED_EDGE('',*,*,#3032,.F.);
#3991=ORIENTED_EDGE('',*,*,#3036,.F.);
#3992=ORIENTED_EDGE('',*,*,#3037,.T.);
#3993=ORIENTED_EDGE('',*,*,#3038,.T.);
#3994=ORIENTED_EDGE('',*,*,#3037,.F.);
#3995=ORIENTED_EDGE('',*,*,#3038,.F.);
#3996=ORIENTED_EDGE('',*,*,#3039,.F.);
#3997=ORIENTED_EDGE('',*,*,#3040,.F.);
#3998=ORIENTED_EDGE('',*,*,#3041,.T.);
#3999=ORIENTED_EDGE('',*,*,#3039,.T.);
#4000=ORIENTED_EDGE('',*,*,#3041,.F.);
#4001=ORIENTED_EDGE('',*,*,#3026,.T.);
#4002=ORIENTED_EDGE('',*,*,#3042,.T.);
#4003=ORIENTED_EDGE('',*,*,#3030,.T.);
#4004=ORIENTED_EDGE('',*,*,#3043,.F.);
#4005=ORIENTED_EDGE('',*,*,#3043,.T.);
#4006=ORIENTED_EDGE('',*,*,#3033,.T.);
#4007=ORIENTED_EDGE('',*,*,#3035,.T.);
#4008=ORIENTED_EDGE('',*,*,#3027,.T.);
#4009=ORIENTED_EDGE('',*,*,#3040,.T.);
#4010=ORIENTED_EDGE('',*,*,#3016,.T.);
#4011=ORIENTED_EDGE('',*,*,#3012,.T.);
#4012=ORIENTED_EDGE('',*,*,#3008,.T.);
#4013=ORIENTED_EDGE('',*,*,#3004,.T.);
#4014=ORIENTED_EDGE('',*,*,#3042,.F.);
#4015=ORIENTED_EDGE('',*,*,#3029,.F.);
#4016=ORIENTED_EDGE('',*,*,#3034,.F.);
#4017=ORIENTED_EDGE('',*,*,#3031,.F.);
#4018=ORIENTED_EDGE('',*,*,#3036,.T.);
#4019=ORIENTED_EDGE('',*,*,#3024,.T.);
#4020=ORIENTED_EDGE('',*,*,#3022,.T.);
#4021=ORIENTED_EDGE('',*,*,#3020,.T.);
#4022=ORIENTED_EDGE('',*,*,#3018,.T.);
#4023=ORIENTED_EDGE('',*,*,#3044,.F.);
#4024=ORIENTED_EDGE('',*,*,#3045,.T.);
#4025=ORIENTED_EDGE('',*,*,#3046,.F.);
#4026=ORIENTED_EDGE('',*,*,#3045,.F.);
#4027=ORIENTED_EDGE('',*,*,#3044,.T.);
#4028=ORIENTED_EDGE('',*,*,#3047,.F.);
#4029=ORIENTED_EDGE('',*,*,#3048,.T.);
#4030=ORIENTED_EDGE('',*,*,#3049,.T.);
#4031=ORIENTED_EDGE('',*,*,#3048,.F.);
#4032=ORIENTED_EDGE('',*,*,#3047,.T.);
#4033=ORIENTED_EDGE('',*,*,#3046,.T.);
#4034=ORIENTED_EDGE('',*,*,#3049,.F.);
#4035=ORIENTED_EDGE('',*,*,#3050,.F.);
#4036=ORIENTED_EDGE('',*,*,#3051,.T.);
#4037=ORIENTED_EDGE('',*,*,#3052,.T.);
#4038=ORIENTED_EDGE('',*,*,#3051,.F.);
#4039=ORIENTED_EDGE('',*,*,#3050,.T.);
#4040=ORIENTED_EDGE('',*,*,#3052,.F.);
#4041=ORIENTED_EDGE('',*,*,#3053,.F.);
#4042=ORIENTED_EDGE('',*,*,#3054,.F.);
#4043=ORIENTED_EDGE('',*,*,#3055,.T.);
#4044=ORIENTED_EDGE('',*,*,#3056,.F.);
#4045=ORIENTED_EDGE('',*,*,#3057,.F.);
#4046=ORIENTED_EDGE('',*,*,#3055,.F.);
#4047=ORIENTED_EDGE('',*,*,#3056,.T.);
#4048=ORIENTED_EDGE('',*,*,#3057,.T.);
#4049=ORIENTED_EDGE('',*,*,#3058,.T.);
#4050=ORIENTED_EDGE('',*,*,#3059,.T.);
#4051=ORIENTED_EDGE('',*,*,#3058,.F.);
#4052=ORIENTED_EDGE('',*,*,#3060,.T.);
#4053=ORIENTED_EDGE('',*,*,#3061,.T.);
#4054=ORIENTED_EDGE('',*,*,#3062,.F.);
#4055=ORIENTED_EDGE('',*,*,#3061,.F.);
#4056=ORIENTED_EDGE('',*,*,#3062,.T.);
#4057=ORIENTED_EDGE('',*,*,#3063,.T.);
#4058=ORIENTED_EDGE('',*,*,#3064,.F.);
#4059=ORIENTED_EDGE('',*,*,#3063,.F.);
#4060=ORIENTED_EDGE('',*,*,#3059,.F.);
#4061=ORIENTED_EDGE('',*,*,#3064,.T.);
#4062=ORIENTED_EDGE('',*,*,#3065,.F.);
#4063=ORIENTED_EDGE('',*,*,#3066,.T.);
#4064=ORIENTED_EDGE('',*,*,#3053,.T.);
#4065=ORIENTED_EDGE('',*,*,#3054,.T.);
#4066=ORIENTED_EDGE('',*,*,#3066,.F.);
#4067=ORIENTED_EDGE('',*,*,#3065,.T.);
#4068=ORIENTED_EDGE('',*,*,#3067,.F.);
#4069=ORIENTED_EDGE('',*,*,#3067,.T.);
#4070=ORIENTED_EDGE('',*,*,#3068,.T.);
#4071=ORIENTED_EDGE('',*,*,#3060,.F.);
#4072=ORIENTED_EDGE('',*,*,#3068,.F.);
#4073=ORIENTED_EDGE('',*,*,#3069,.F.);
#4074=ORIENTED_EDGE('',*,*,#3070,.F.);
#4075=ORIENTED_EDGE('',*,*,#3071,.T.);
#4076=ORIENTED_EDGE('',*,*,#3072,.F.);
#4077=ORIENTED_EDGE('',*,*,#3073,.F.);
#4078=ORIENTED_EDGE('',*,*,#3071,.F.);
#4079=ORIENTED_EDGE('',*,*,#3074,.T.);
#4080=ORIENTED_EDGE('',*,*,#3075,.T.);
#4081=ORIENTED_EDGE('',*,*,#3072,.T.);
#4082=ORIENTED_EDGE('',*,*,#3073,.T.);
#4083=ORIENTED_EDGE('',*,*,#3075,.F.);
#4084=ORIENTED_EDGE('',*,*,#3076,.F.);
#4085=ORIENTED_EDGE('',*,*,#3077,.T.);
#4086=ORIENTED_EDGE('',*,*,#3078,.F.);
#4087=ORIENTED_EDGE('',*,*,#3079,.T.);
#4088=ORIENTED_EDGE('',*,*,#3076,.T.);
#4089=ORIENTED_EDGE('',*,*,#3079,.F.);
#4090=ORIENTED_EDGE('',*,*,#3080,.F.);
#4091=ORIENTED_EDGE('',*,*,#3081,.T.);
#4092=ORIENTED_EDGE('',*,*,#3078,.T.);
#4093=ORIENTED_EDGE('',*,*,#3081,.F.);
#4094=ORIENTED_EDGE('',*,*,#3082,.F.);
#4095=ORIENTED_EDGE('',*,*,#3083,.T.);
#4096=ORIENTED_EDGE('',*,*,#3080,.T.);
#4097=ORIENTED_EDGE('',*,*,#3083,.F.);
#4098=ORIENTED_EDGE('',*,*,#3082,.T.);
#4099=ORIENTED_EDGE('',*,*,#3074,.F.);
#4100=ORIENTED_EDGE('',*,*,#3069,.T.);
#4101=ORIENTED_EDGE('',*,*,#3070,.T.);
#4102=ORIENTED_EDGE('',*,*,#3084,.T.);
#4103=ORIENTED_EDGE('',*,*,#3077,.F.);
#4104=ORIENTED_EDGE('',*,*,#3084,.F.);
#4105=ORIENTED_EDGE('',*,*,#3085,.T.);
#4106=ORIENTED_EDGE('',*,*,#3085,.F.);
#4107=ORIENTED_EDGE('',*,*,#3086,.T.);
#4108=ORIENTED_EDGE('',*,*,#3086,.F.);
#4109=ORIENTED_EDGE('',*,*,#3087,.T.);
#4110=ORIENTED_EDGE('',*,*,#3087,.F.);
#4111=ORIENTED_EDGE('',*,*,#3088,.T.);
#4112=ORIENTED_EDGE('',*,*,#3088,.F.);
#4113=ORIENTED_EDGE('',*,*,#3089,.T.);
#4114=ORIENTED_EDGE('',*,*,#3089,.F.);
#4115=ORIENTED_EDGE('',*,*,#3090,.T.);
#4116=ORIENTED_EDGE('',*,*,#3090,.F.);
#4117=ORIENTED_EDGE('',*,*,#3091,.T.);
#4118=ORIENTED_EDGE('',*,*,#3091,.F.);
#4119=ORIENTED_EDGE('',*,*,#3092,.T.);
#4120=ORIENTED_EDGE('',*,*,#3092,.F.);
#4121=ORIENTED_EDGE('',*,*,#3093,.F.);
#4122=ORIENTED_EDGE('',*,*,#3094,.F.);
#4123=ORIENTED_EDGE('',*,*,#3095,.F.);
#4124=ORIENTED_EDGE('',*,*,#3096,.F.);
#4125=ORIENTED_EDGE('',*,*,#3095,.T.);
#4126=ORIENTED_EDGE('',*,*,#3097,.F.);
#4127=ORIENTED_EDGE('',*,*,#3098,.T.);
#4128=ORIENTED_EDGE('',*,*,#3099,.F.);
#4129=ORIENTED_EDGE('',*,*,#3100,.T.);
#4130=ORIENTED_EDGE('',*,*,#3101,.F.);
#4131=ORIENTED_EDGE('',*,*,#3102,.T.);
#4132=ORIENTED_EDGE('',*,*,#3103,.T.);
#4133=ORIENTED_EDGE('',*,*,#3104,.F.);
#4134=ORIENTED_EDGE('',*,*,#3103,.F.);
#4135=ORIENTED_EDGE('',*,*,#3105,.T.);
#4136=ORIENTED_EDGE('',*,*,#3106,.F.);
#4137=ORIENTED_EDGE('',*,*,#3107,.T.);
#4138=ORIENTED_EDGE('',*,*,#3108,.F.);
#4139=ORIENTED_EDGE('',*,*,#3109,.T.);
#4140=ORIENTED_EDGE('',*,*,#3110,.F.);
#4141=ORIENTED_EDGE('',*,*,#3111,.T.);
#4142=ORIENTED_EDGE('',*,*,#3112,.F.);
#4143=ORIENTED_EDGE('',*,*,#3113,.T.);
#4144=ORIENTED_EDGE('',*,*,#3114,.F.);
#4145=ORIENTED_EDGE('',*,*,#3094,.T.);
#4146=ORIENTED_EDGE('',*,*,#3115,.T.);
#4147=ORIENTED_EDGE('',*,*,#3116,.T.);
#4148=ORIENTED_EDGE('',*,*,#3097,.T.);
#4149=ORIENTED_EDGE('',*,*,#3117,.F.);
#4150=ORIENTED_EDGE('',*,*,#3118,.F.);
#4151=ORIENTED_EDGE('',*,*,#3098,.F.);
#4152=ORIENTED_EDGE('',*,*,#3116,.F.);
#4153=ORIENTED_EDGE('',*,*,#3118,.T.);
#4154=ORIENTED_EDGE('',*,*,#3119,.T.);
#4155=ORIENTED_EDGE('',*,*,#3120,.T.);
#4156=ORIENTED_EDGE('',*,*,#3099,.T.);
#4157=ORIENTED_EDGE('',*,*,#3121,.F.);
#4158=ORIENTED_EDGE('',*,*,#3122,.F.);
#4159=ORIENTED_EDGE('',*,*,#3100,.F.);
#4160=ORIENTED_EDGE('',*,*,#3120,.F.);
#4161=ORIENTED_EDGE('',*,*,#3122,.T.);
#4162=ORIENTED_EDGE('',*,*,#3123,.T.);
#4163=ORIENTED_EDGE('',*,*,#3124,.T.);
#4164=ORIENTED_EDGE('',*,*,#3101,.T.);
#4165=ORIENTED_EDGE('',*,*,#3125,.F.);
#4166=ORIENTED_EDGE('',*,*,#3126,.F.);
#4167=ORIENTED_EDGE('',*,*,#3105,.F.);
#4168=ORIENTED_EDGE('',*,*,#3102,.F.);
#4169=ORIENTED_EDGE('',*,*,#3124,.F.);
#4170=ORIENTED_EDGE('',*,*,#3127,.F.);
#4171=ORIENTED_EDGE('',*,*,#3126,.T.);
#4172=ORIENTED_EDGE('',*,*,#3128,.T.);
#4173=ORIENTED_EDGE('',*,*,#3129,.T.);
#4174=ORIENTED_EDGE('',*,*,#3106,.T.);
#4175=ORIENTED_EDGE('',*,*,#3130,.F.);
#4176=ORIENTED_EDGE('',*,*,#3131,.F.);
#4177=ORIENTED_EDGE('',*,*,#3107,.F.);
#4178=ORIENTED_EDGE('',*,*,#3129,.F.);
#4179=ORIENTED_EDGE('',*,*,#3131,.T.);
#4180=ORIENTED_EDGE('',*,*,#3132,.T.);
#4181=ORIENTED_EDGE('',*,*,#3133,.T.);
#4182=ORIENTED_EDGE('',*,*,#3108,.T.);
#4183=ORIENTED_EDGE('',*,*,#3134,.F.);
#4184=ORIENTED_EDGE('',*,*,#3135,.F.);
#4185=ORIENTED_EDGE('',*,*,#3109,.F.);
#4186=ORIENTED_EDGE('',*,*,#3133,.F.);
#4187=ORIENTED_EDGE('',*,*,#3135,.T.);
#4188=ORIENTED_EDGE('',*,*,#3136,.T.);
#4189=ORIENTED_EDGE('',*,*,#3137,.T.);
#4190=ORIENTED_EDGE('',*,*,#3110,.T.);
#4191=ORIENTED_EDGE('',*,*,#3111,.F.);
#4192=ORIENTED_EDGE('',*,*,#3137,.F.);
#4193=ORIENTED_EDGE('',*,*,#3138,.F.);
#4194=ORIENTED_EDGE('',*,*,#3139,.F.);
#4195=ORIENTED_EDGE('',*,*,#3140,.F.);
#4196=ORIENTED_EDGE('',*,*,#3141,.T.);
#4197=ORIENTED_EDGE('',*,*,#3127,.T.);
#4198=ORIENTED_EDGE('',*,*,#3123,.F.);
#4199=ORIENTED_EDGE('',*,*,#3121,.T.);
#4200=ORIENTED_EDGE('',*,*,#3119,.F.);
#4201=ORIENTED_EDGE('',*,*,#3117,.T.);
#4202=ORIENTED_EDGE('',*,*,#3115,.F.);
#4203=ORIENTED_EDGE('',*,*,#3093,.T.);
#4204=ORIENTED_EDGE('',*,*,#3142,.F.);
#4205=ORIENTED_EDGE('',*,*,#3143,.T.);
#4206=ORIENTED_EDGE('',*,*,#3144,.F.);
#4207=ORIENTED_EDGE('',*,*,#3138,.T.);
#4208=ORIENTED_EDGE('',*,*,#3136,.F.);
#4209=ORIENTED_EDGE('',*,*,#3134,.T.);
#4210=ORIENTED_EDGE('',*,*,#3132,.F.);
#4211=ORIENTED_EDGE('',*,*,#3130,.T.);
#4212=ORIENTED_EDGE('',*,*,#3128,.F.);
#4213=ORIENTED_EDGE('',*,*,#3125,.T.);
#4214=ORIENTED_EDGE('',*,*,#3141,.F.);
#4215=ORIENTED_EDGE('',*,*,#3096,.T.);
#4216=ORIENTED_EDGE('',*,*,#3114,.T.);
#4217=ORIENTED_EDGE('',*,*,#3145,.T.);
#4218=ORIENTED_EDGE('',*,*,#3142,.T.);
#4219=ORIENTED_EDGE('',*,*,#3113,.F.);
#4220=ORIENTED_EDGE('',*,*,#3146,.F.);
#4221=ORIENTED_EDGE('',*,*,#3143,.F.);
#4222=ORIENTED_EDGE('',*,*,#3145,.F.);
#4223=ORIENTED_EDGE('',*,*,#3104,.T.);
#4224=ORIENTED_EDGE('',*,*,#3140,.T.);
#4225=ORIENTED_EDGE('',*,*,#3139,.T.);
#4226=ORIENTED_EDGE('',*,*,#3144,.T.);
#4227=ORIENTED_EDGE('',*,*,#3146,.T.);
#4228=ORIENTED_EDGE('',*,*,#3112,.T.);
#4229=ORIENTED_EDGE('',*,*,#3147,.F.);
#4230=ORIENTED_EDGE('',*,*,#3148,.T.);
#4231=ORIENTED_EDGE('',*,*,#3149,.F.);
#4232=ORIENTED_EDGE('',*,*,#3150,.T.);
#4233=ORIENTED_EDGE('',*,*,#3147,.T.);
#4234=ORIENTED_EDGE('',*,*,#3150,.F.);
#4235=ORIENTED_EDGE('',*,*,#3149,.T.);
#4236=ORIENTED_EDGE('',*,*,#3151,.F.);
#4237=ORIENTED_EDGE('',*,*,#3151,.T.);
#4238=ORIENTED_EDGE('',*,*,#3152,.T.);
#4239=ORIENTED_EDGE('',*,*,#3148,.F.);
#4240=ORIENTED_EDGE('',*,*,#3152,.F.);
#4241=ORIENTED_EDGE('',*,*,#3153,.F.);
#4242=ORIENTED_EDGE('',*,*,#3154,.T.);
#4243=ORIENTED_EDGE('',*,*,#3155,.F.);
#4244=ORIENTED_EDGE('',*,*,#3156,.T.);
#4245=ORIENTED_EDGE('',*,*,#3153,.T.);
#4246=ORIENTED_EDGE('',*,*,#3156,.F.);
#4247=ORIENTED_EDGE('',*,*,#3155,.T.);
#4248=ORIENTED_EDGE('',*,*,#3157,.F.);
#4249=ORIENTED_EDGE('',*,*,#3157,.T.);
#4250=ORIENTED_EDGE('',*,*,#3158,.T.);
#4251=ORIENTED_EDGE('',*,*,#3154,.F.);
#4252=ORIENTED_EDGE('',*,*,#3158,.F.);
#4253=ORIENTED_EDGE('',*,*,#3159,.F.);
#4254=ORIENTED_EDGE('',*,*,#3160,.T.);
#4255=ORIENTED_EDGE('',*,*,#3161,.F.);
#4256=ORIENTED_EDGE('',*,*,#3160,.F.);
#4257=ORIENTED_EDGE('',*,*,#3159,.T.);
#4258=ORIENTED_EDGE('',*,*,#3162,.F.);
#4259=ORIENTED_EDGE('',*,*,#3163,.T.);
#4260=ORIENTED_EDGE('',*,*,#3164,.T.);
#4261=ORIENTED_EDGE('',*,*,#3163,.F.);
#4262=ORIENTED_EDGE('',*,*,#3164,.F.);
#4263=ORIENTED_EDGE('',*,*,#3165,.T.);
#4264=ORIENTED_EDGE('',*,*,#3166,.F.);
#4265=ORIENTED_EDGE('',*,*,#3165,.F.);
#4266=ORIENTED_EDGE('',*,*,#3167,.T.);
#4267=ORIENTED_EDGE('',*,*,#3168,.F.);
#4268=ORIENTED_EDGE('',*,*,#3167,.F.);
#4269=ORIENTED_EDGE('',*,*,#3169,.F.);
#4270=ORIENTED_EDGE('',*,*,#3170,.F.);
#4271=ORIENTED_EDGE('',*,*,#3171,.F.);
#4272=ORIENTED_EDGE('',*,*,#3172,.T.);
#4273=ORIENTED_EDGE('',*,*,#3169,.T.);
#4274=ORIENTED_EDGE('',*,*,#3172,.F.);
#4275=ORIENTED_EDGE('',*,*,#3170,.T.);
#4276=ORIENTED_EDGE('',*,*,#3173,.T.);
#4277=ORIENTED_EDGE('',*,*,#3174,.T.);
#4278=ORIENTED_EDGE('',*,*,#3173,.F.);
#4279=ORIENTED_EDGE('',*,*,#3175,.F.);
#4280=ORIENTED_EDGE('',*,*,#3176,.T.);
#4281=ORIENTED_EDGE('',*,*,#3166,.T.);
#4282=ORIENTED_EDGE('',*,*,#3176,.F.);
#4283=ORIENTED_EDGE('',*,*,#3175,.T.);
#4284=ORIENTED_EDGE('',*,*,#3161,.T.);
#4285=ORIENTED_EDGE('',*,*,#3174,.F.);
#4286=ORIENTED_EDGE('',*,*,#3162,.T.);
#4287=ORIENTED_EDGE('',*,*,#3177,.F.);
#4288=ORIENTED_EDGE('',*,*,#3178,.T.);
#4289=ORIENTED_EDGE('',*,*,#3179,.T.);
#4290=ORIENTED_EDGE('',*,*,#3178,.F.);
#4291=ORIENTED_EDGE('',*,*,#3177,.T.);
#4292=ORIENTED_EDGE('',*,*,#3168,.T.);
#4293=ORIENTED_EDGE('',*,*,#3179,.F.);
#4294=ORIENTED_EDGE('',*,*,#3171,.T.);
#4295=ORIENTED_EDGE('',*,*,#3180,.F.);
#4296=ORIENTED_EDGE('',*,*,#3181,.T.);
#4297=ORIENTED_EDGE('',*,*,#3182,.F.);
#4298=ORIENTED_EDGE('',*,*,#3181,.F.);
#4299=ORIENTED_EDGE('',*,*,#3183,.F.);
#4300=ORIENTED_EDGE('',*,*,#3184,.F.);
#4301=ORIENTED_EDGE('',*,*,#3185,.F.);
#4302=ORIENTED_EDGE('',*,*,#3186,.T.);
#4303=ORIENTED_EDGE('',*,*,#3186,.F.);
#4304=ORIENTED_EDGE('',*,*,#3187,.T.);
#4305=ORIENTED_EDGE('',*,*,#3188,.F.);
#4306=ORIENTED_EDGE('',*,*,#3189,.F.);
#4307=ORIENTED_EDGE('',*,*,#3190,.T.);
#4308=ORIENTED_EDGE('',*,*,#3180,.T.);
#4309=ORIENTED_EDGE('',*,*,#3191,.F.);
#4310=ORIENTED_EDGE('',*,*,#3185,.T.);
#4311=ORIENTED_EDGE('',*,*,#3192,.F.);
#4312=ORIENTED_EDGE('',*,*,#3193,.F.);
#4313=ORIENTED_EDGE('',*,*,#3187,.F.);
#4314=ORIENTED_EDGE('',*,*,#3183,.T.);
#4315=ORIENTED_EDGE('',*,*,#3190,.F.);
#4316=ORIENTED_EDGE('',*,*,#3194,.F.);
#4317=ORIENTED_EDGE('',*,*,#3195,.F.);
#4318=ORIENTED_EDGE('',*,*,#3195,.T.);
#4319=ORIENTED_EDGE('',*,*,#3196,.F.);
#4320=ORIENTED_EDGE('',*,*,#3192,.T.);
#4321=ORIENTED_EDGE('',*,*,#3184,.T.);
#4322=ORIENTED_EDGE('',*,*,#3182,.T.);
#4323=ORIENTED_EDGE('',*,*,#3197,.F.);
#4324=ORIENTED_EDGE('',*,*,#3198,.T.);
#4325=ORIENTED_EDGE('',*,*,#3191,.T.);
#4326=ORIENTED_EDGE('',*,*,#3198,.F.);
#4327=ORIENTED_EDGE('',*,*,#3199,.F.);
#4328=ORIENTED_EDGE('',*,*,#3200,.T.);
#4329=ORIENTED_EDGE('',*,*,#3188,.T.);
#4330=ORIENTED_EDGE('',*,*,#3193,.T.);
#4331=ORIENTED_EDGE('',*,*,#3196,.T.);
#4332=ORIENTED_EDGE('',*,*,#3194,.T.);
#4333=ORIENTED_EDGE('',*,*,#3189,.T.);
#4334=ORIENTED_EDGE('',*,*,#3200,.F.);
#4335=ORIENTED_EDGE('',*,*,#3199,.T.);
#4336=ORIENTED_EDGE('',*,*,#3197,.T.);
#4337=ORIENTED_EDGE('',*,*,#3201,.F.);
#4338=ORIENTED_EDGE('',*,*,#3202,.T.);
#4339=ORIENTED_EDGE('',*,*,#3203,.F.);
#4340=ORIENTED_EDGE('',*,*,#3202,.F.);
#4341=ORIENTED_EDGE('',*,*,#3201,.T.);
#4342=ORIENTED_EDGE('',*,*,#3204,.F.);
#4343=ORIENTED_EDGE('',*,*,#3205,.T.);
#4344=ORIENTED_EDGE('',*,*,#3206,.T.);
#4345=ORIENTED_EDGE('',*,*,#3205,.F.);
#4346=ORIENTED_EDGE('',*,*,#3204,.T.);
#4347=ORIENTED_EDGE('',*,*,#3203,.T.);
#4348=ORIENTED_EDGE('',*,*,#3206,.F.);
#4349=ORIENTED_EDGE('',*,*,#3207,.F.);
#4350=ORIENTED_EDGE('',*,*,#3208,.T.);
#4351=ORIENTED_EDGE('',*,*,#3209,.T.);
#4352=ORIENTED_EDGE('',*,*,#3208,.F.);
#4353=ORIENTED_EDGE('',*,*,#3210,.F.);
#4354=ORIENTED_EDGE('',*,*,#3211,.T.);
#4355=ORIENTED_EDGE('',*,*,#3212,.T.);
#4356=ORIENTED_EDGE('',*,*,#3211,.F.);
#4357=ORIENTED_EDGE('',*,*,#3210,.T.);
#4358=ORIENTED_EDGE('',*,*,#3207,.T.);
#4359=ORIENTED_EDGE('',*,*,#3212,.F.);
#4360=ORIENTED_EDGE('',*,*,#3209,.F.);
#4361=ORIENTED_EDGE('',*,*,#3213,.F.);
#4362=ORIENTED_EDGE('',*,*,#3214,.T.);
#4363=ORIENTED_EDGE('',*,*,#3215,.T.);
#4364=ORIENTED_EDGE('',*,*,#3214,.F.);
#4365=ORIENTED_EDGE('',*,*,#3216,.F.);
#4366=ORIENTED_EDGE('',*,*,#3217,.T.);
#4367=ORIENTED_EDGE('',*,*,#3218,.T.);
#4368=ORIENTED_EDGE('',*,*,#3217,.F.);
#4369=ORIENTED_EDGE('',*,*,#3216,.T.);
#4370=ORIENTED_EDGE('',*,*,#3213,.T.);
#4371=ORIENTED_EDGE('',*,*,#3218,.F.);
#4372=ORIENTED_EDGE('',*,*,#3215,.F.);
#4373=ORIENTED_EDGE('',*,*,#3219,.F.);
#4374=ORIENTED_EDGE('',*,*,#3220,.F.);
#4375=ORIENTED_EDGE('',*,*,#3221,.T.);
#4376=ORIENTED_EDGE('',*,*,#3219,.T.);
#4377=ORIENTED_EDGE('',*,*,#3221,.F.);
#4378=ORIENTED_EDGE('',*,*,#3222,.F.);
#4379=ORIENTED_EDGE('',*,*,#3223,.T.);
#4380=ORIENTED_EDGE('',*,*,#3220,.T.);
#4381=ORIENTED_EDGE('',*,*,#3223,.F.);
#4382=ORIENTED_EDGE('',*,*,#3224,.F.);
#4383=ORIENTED_EDGE('',*,*,#3225,.T.);
#4384=ORIENTED_EDGE('',*,*,#3222,.T.);
#4385=ORIENTED_EDGE('',*,*,#3225,.F.);
#4386=ORIENTED_EDGE('',*,*,#3224,.T.);
#4387=ORIENTED_EDGE('',*,*,#3226,.F.);
#4388=ORIENTED_EDGE('',*,*,#3227,.F.);
#4389=ORIENTED_EDGE('',*,*,#3228,.T.);
#4390=ORIENTED_EDGE('',*,*,#3226,.T.);
#4391=ORIENTED_EDGE('',*,*,#3228,.F.);
#4392=ORIENTED_EDGE('',*,*,#3229,.F.);
#4393=ORIENTED_EDGE('',*,*,#3230,.T.);
#4394=ORIENTED_EDGE('',*,*,#3227,.T.);
#4395=ORIENTED_EDGE('',*,*,#3230,.F.);
#4396=ORIENTED_EDGE('',*,*,#3231,.F.);
#4397=ORIENTED_EDGE('',*,*,#3232,.T.);
#4398=ORIENTED_EDGE('',*,*,#3229,.T.);
#4399=ORIENTED_EDGE('',*,*,#3232,.F.);
#4400=ORIENTED_EDGE('',*,*,#3231,.T.);
#4401=ORIENTED_EDGE('',*,*,#3233,.T.);
#4402=ORIENTED_EDGE('',*,*,#3234,.T.);
#4403=ORIENTED_EDGE('',*,*,#3235,.T.);
#4404=ORIENTED_EDGE('',*,*,#3236,.F.);
#4405=ORIENTED_EDGE('',*,*,#3237,.T.);
#4406=ORIENTED_EDGE('',*,*,#3238,.T.);
#4407=ORIENTED_EDGE('',*,*,#3239,.T.);
#4408=ORIENTED_EDGE('',*,*,#3234,.F.);
#4409=ORIENTED_EDGE('',*,*,#3240,.T.);
#4410=ORIENTED_EDGE('',*,*,#3241,.T.);
#4411=ORIENTED_EDGE('',*,*,#3242,.T.);
#4412=ORIENTED_EDGE('',*,*,#3238,.F.);
#4413=ORIENTED_EDGE('',*,*,#3243,.T.);
#4414=ORIENTED_EDGE('',*,*,#3244,.T.);
#4415=ORIENTED_EDGE('',*,*,#3245,.T.);
#4416=ORIENTED_EDGE('',*,*,#3241,.F.);
#4417=ORIENTED_EDGE('',*,*,#3246,.T.);
#4418=ORIENTED_EDGE('',*,*,#3247,.T.);
#4419=ORIENTED_EDGE('',*,*,#3248,.T.);
#4420=ORIENTED_EDGE('',*,*,#3244,.F.);
#4421=ORIENTED_EDGE('',*,*,#3249,.T.);
#4422=ORIENTED_EDGE('',*,*,#3236,.T.);
#4423=ORIENTED_EDGE('',*,*,#3250,.T.);
#4424=ORIENTED_EDGE('',*,*,#3247,.F.);
#4425=ORIENTED_EDGE('',*,*,#3249,.F.);
#4426=ORIENTED_EDGE('',*,*,#3246,.F.);
#4427=ORIENTED_EDGE('',*,*,#3243,.F.);
#4428=ORIENTED_EDGE('',*,*,#3240,.F.);
#4429=ORIENTED_EDGE('',*,*,#3237,.F.);
#4430=ORIENTED_EDGE('',*,*,#3233,.F.);
#4431=ORIENTED_EDGE('',*,*,#3250,.F.);
#4432=ORIENTED_EDGE('',*,*,#3235,.F.);
#4433=ORIENTED_EDGE('',*,*,#3239,.F.);
#4434=ORIENTED_EDGE('',*,*,#3242,.F.);
#4435=ORIENTED_EDGE('',*,*,#3245,.F.);
#4436=ORIENTED_EDGE('',*,*,#3248,.F.);
#4437=ORIENTED_EDGE('',*,*,#3251,.T.);
#4438=ORIENTED_EDGE('',*,*,#3252,.T.);
#4439=ORIENTED_EDGE('',*,*,#3253,.T.);
#4440=ORIENTED_EDGE('',*,*,#3254,.F.);
#4441=ORIENTED_EDGE('',*,*,#3255,.T.);
#4442=ORIENTED_EDGE('',*,*,#3256,.T.);
#4443=ORIENTED_EDGE('',*,*,#3257,.T.);
#4444=ORIENTED_EDGE('',*,*,#3252,.F.);
#4445=ORIENTED_EDGE('',*,*,#3258,.T.);
#4446=ORIENTED_EDGE('',*,*,#3259,.T.);
#4447=ORIENTED_EDGE('',*,*,#3260,.T.);
#4448=ORIENTED_EDGE('',*,*,#3256,.F.);
#4449=ORIENTED_EDGE('',*,*,#3261,.T.);
#4450=ORIENTED_EDGE('',*,*,#3262,.T.);
#4451=ORIENTED_EDGE('',*,*,#3263,.T.);
#4452=ORIENTED_EDGE('',*,*,#3259,.F.);
#4453=ORIENTED_EDGE('',*,*,#3264,.T.);
#4454=ORIENTED_EDGE('',*,*,#3265,.T.);
#4455=ORIENTED_EDGE('',*,*,#3266,.T.);
#4456=ORIENTED_EDGE('',*,*,#3262,.F.);
#4457=ORIENTED_EDGE('',*,*,#3267,.T.);
#4458=ORIENTED_EDGE('',*,*,#3254,.T.);
#4459=ORIENTED_EDGE('',*,*,#3268,.T.);
#4460=ORIENTED_EDGE('',*,*,#3265,.F.);
#4461=ORIENTED_EDGE('',*,*,#3267,.F.);
#4462=ORIENTED_EDGE('',*,*,#3264,.F.);
#4463=ORIENTED_EDGE('',*,*,#3261,.F.);
#4464=ORIENTED_EDGE('',*,*,#3258,.F.);
#4465=ORIENTED_EDGE('',*,*,#3255,.F.);
#4466=ORIENTED_EDGE('',*,*,#3251,.F.);
#4467=ORIENTED_EDGE('',*,*,#3268,.F.);
#4468=ORIENTED_EDGE('',*,*,#3253,.F.);
#4469=ORIENTED_EDGE('',*,*,#3257,.F.);
#4470=ORIENTED_EDGE('',*,*,#3260,.F.);
#4471=ORIENTED_EDGE('',*,*,#3263,.F.);
#4472=ORIENTED_EDGE('',*,*,#3266,.F.);
#4473=ORIENTED_EDGE('',*,*,#3269,.F.);
#4474=ORIENTED_EDGE('',*,*,#3270,.F.);
#4475=ORIENTED_EDGE('',*,*,#3271,.F.);
#4476=ORIENTED_EDGE('',*,*,#3272,.T.);
#4477=ORIENTED_EDGE('',*,*,#3270,.T.);
#4478=ORIENTED_EDGE('',*,*,#3272,.F.);
#4479=ORIENTED_EDGE('',*,*,#3273,.F.);
#4480=ORIENTED_EDGE('',*,*,#3274,.T.);
#4481=ORIENTED_EDGE('',*,*,#3271,.T.);
#4482=ORIENTED_EDGE('',*,*,#3274,.F.);
#4483=ORIENTED_EDGE('',*,*,#3275,.F.);
#4484=ORIENTED_EDGE('',*,*,#3276,.T.);
#4485=ORIENTED_EDGE('',*,*,#3273,.T.);
#4486=ORIENTED_EDGE('',*,*,#3276,.F.);
#4487=ORIENTED_EDGE('',*,*,#3275,.T.);
#4488=ORIENTED_EDGE('',*,*,#3277,.F.);
#4489=ORIENTED_EDGE('',*,*,#3278,.F.);
#4490=ORIENTED_EDGE('',*,*,#3279,.T.);
#4491=ORIENTED_EDGE('',*,*,#3277,.T.);
#4492=ORIENTED_EDGE('',*,*,#3279,.F.);
#4493=ORIENTED_EDGE('',*,*,#3269,.T.);
#4494=ORIENTED_EDGE('',*,*,#3280,.T.);
#4495=ORIENTED_EDGE('',*,*,#3278,.T.);
#4496=ORIENTED_EDGE('',*,*,#3280,.F.);
#4497=CYLINDRICAL_SURFACE('',#5226,0.21);
#4498=CYLINDRICAL_SURFACE('',#5229,0.21);
#4499=CYLINDRICAL_SURFACE('',#5232,0.21);
#4500=CYLINDRICAL_SURFACE('',#5235,0.21);
#4501=CYLINDRICAL_SURFACE('',#5263,0.5);
#4502=CYLINDRICAL_SURFACE('',#5269,0.5);
#4503=CYLINDRICAL_SURFACE('',#5275,0.5);
#4504=CYLINDRICAL_SURFACE('',#5281,0.5);
#4505=CYLINDRICAL_SURFACE('',#5290,1.8);
#4506=CYLINDRICAL_SURFACE('',#5292,0.3);
#4507=CYLINDRICAL_SURFACE('',#5309,0.5);
#4508=CYLINDRICAL_SURFACE('',#5315,0.305);
#4509=CYLINDRICAL_SURFACE('',#5329,0.305);
#4510=CYLINDRICAL_SURFACE('',#5343,0.275);
#4511=CYLINDRICAL_SURFACE('',#5345,0.275);
#4512=CYLINDRICAL_SURFACE('',#5347,0.275);
#4513=CYLINDRICAL_SURFACE('',#5349,0.275);
#4514=CYLINDRICAL_SURFACE('',#5354,0.7);
#4515=CYLINDRICAL_SURFACE('',#5357,0.5);
#4516=CYLINDRICAL_SURFACE('',#5386,0.425);
#4517=CYLINDRICAL_SURFACE('',#5394,0.24505);
#4518=CYLINDRICAL_SURFACE('',#5407,0.165);
#4519=CYLINDRICAL_SURFACE('',#5411,0.165);
#4520=CYLINDRICAL_SURFACE('',#5415,0.165);
#4521=CYLINDRICAL_SURFACE('',#5419,0.165);
#4522=CYLINDRICAL_SURFACE('',#5423,0.165);
#4523=CYLINDRICAL_SURFACE('',#5427,0.165);
#4524=CYLINDRICAL_SURFACE('',#5431,0.165);
#4525=CYLINDRICAL_SURFACE('',#5435,0.165);
#4526=CYLINDRICAL_SURFACE('',#5439,0.25);
#4527=CYLINDRICAL_SURFACE('',#5443,1.4);
#4528=CYLINDRICAL_SURFACE('',#5452,1.5);
#4529=CYLINDRICAL_SURFACE('',#5455,2.2);
#4530=CYLINDRICAL_SURFACE('',#5461,1.02);
#4531=CYLINDRICAL_SURFACE('',#5464,1.49);
#4532=CYLINDRICAL_SURFACE('',#5470,0.505);
#4533=CYLINDRICAL_SURFACE('',#5473,0.7);
#4534=CYLINDRICAL_SURFACE('',#5479,0.375);
#4535=CYLINDRICAL_SURFACE('',#5484,0.375);
#4536=CYLINDRICAL_SURFACE('',#5489,0.375);
#4537=CYLINDRICAL_SURFACE('',#5494,0.375);
#4538=CYLINDRICAL_SURFACE('',#5499,0.225);
#4539=CYLINDRICAL_SURFACE('',#5501,0.225);
#4540=CYLINDRICAL_SURFACE('',#5503,0.225);
#4541=CYLINDRICAL_SURFACE('',#5505,0.225);
#4542=CYLINDRICAL_SURFACE('',#5507,1.49);
#4543=CYLINDRICAL_SURFACE('',#5512,0.71);
#4544=CYLINDRICAL_SURFACE('',#5514,2.2);
#4545=CYLINDRICAL_SURFACE('',#5520,0.375);
#4546=CYLINDRICAL_SURFACE('',#5525,0.375);
#4547=CYLINDRICAL_SURFACE('',#5530,0.375);
#4548=CYLINDRICAL_SURFACE('',#5535,0.375);
#4549=CYLINDRICAL_SURFACE('',#5540,0.225);
#4550=CYLINDRICAL_SURFACE('',#5542,0.225);
#4551=CYLINDRICAL_SURFACE('',#5544,0.225);
#4552=CYLINDRICAL_SURFACE('',#5546,0.225);
#4553=CYLINDRICAL_SURFACE('',#5551,1.49);
#4554=CYLINDRICAL_SURFACE('',#5556,0.71);
#4555=CYLINDRICAL_SURFACE('',#5558,2.2);
#4556=CYLINDRICAL_SURFACE('',#5564,0.300000000000001);
#4557=CYLINDRICAL_SURFACE('',#5568,1.2);
#4558=CYLINDRICAL_SURFACE('',#5574,1.2);
#4559=CYLINDRICAL_SURFACE('',#5587,0.976185);
#4560=CYLINDRICAL_SURFACE('',#5589,0.5);
#4561=CYLINDRICAL_SURFACE('',#5595,0.976185);
#4562=CYLINDRICAL_SURFACE('',#5607,1.023815);
#4563=CYLINDRICAL_SURFACE('',#5614,1.5);
#4564=CYLINDRICAL_SURFACE('',#5619,1.023815);
#4565=CYLINDRICAL_SURFACE('',#5641,1.019052);
#4566=CYLINDRICAL_SURFACE('',#5681,0.980948);
#4567=CYLINDRICAL_SURFACE('',#5695,1.013815);
#4568=CYLINDRICAL_SURFACE('',#5699,0.991185);
#4569=CYLINDRICAL_SURFACE('',#5703,1.013815);
#4570=CYLINDRICAL_SURFACE('',#5707,0.991185);
#4571=CYLINDRICAL_SURFACE('',#5715,0.165);
#4572=CYLINDRICAL_SURFACE('',#5719,0.165);
#4573=CYLINDRICAL_SURFACE('',#5726,0.5);
#4574=CYLINDRICAL_SURFACE('',#5731,0.5);
#4575=CYLINDRICAL_SURFACE('',#5733,0.3);
#4576=CYLINDRICAL_SURFACE('',#5735,0.3);
#4577=CYLINDRICAL_SURFACE('',#5739,1.2);
#4578=CYLINDRICAL_SURFACE('',#5745,0.225);
#4579=CYLINDRICAL_SURFACE('',#5748,0.699999999999999);
#4580=CYLINDRICAL_SURFACE('',#5759,0.3);
#4581=CYLINDRICAL_SURFACE('',#5761,0.7);
#4582=CYLINDRICAL_SURFACE('',#5765,0.164999999999999);
#4583=CYLINDRICAL_SURFACE('',#5769,0.6);
#4584=CYLINDRICAL_SURFACE('',#5775,0.225);
#4585=CYLINDRICAL_SURFACE('',#5778,0.6);
#4586=CYLINDRICAL_SURFACE('',#5784,0.225);
#4587=CYLINDRICAL_SURFACE('',#5787,0.6);
#4588=CYLINDRICAL_SURFACE('',#5797,0.35);
#4589=CYLINDRICAL_SURFACE('',#5805,0.1954);
#4590=CYLINDRICAL_SURFACE('',#5833,0.35);
#4591=CYLINDRICAL_SURFACE('',#5841,0.1954);
#4592=ADVANCED_FACE('',(#637),#4497,.F.);
#4593=ADVANCED_FACE('',(#638),#4498,.F.);
#4594=ADVANCED_FACE('',(#639),#4499,.F.);
#4595=ADVANCED_FACE('',(#640),#4500,.F.);
#4596=ADVANCED_FACE('',(#641),#458,.T.);
#4597=ADVANCED_FACE('',(#642),#459,.T.);
#4598=ADVANCED_FACE('',(#643),#460,.T.);
#4599=ADVANCED_FACE('',(#644),#461,.T.);
#4600=ADVANCED_FACE('',(#645,#358,#359,#360,#361),#462,.T.);
#4601=ADVANCED_FACE('',(#646,#362,#363,#364,#365),#463,.F.);
#4602=ADVANCED_FACE('',(#647),#464,.T.);
#4603=ADVANCED_FACE('',(#648),#465,.T.);
#4604=ADVANCED_FACE('',(#649),#466,.T.);
#4605=ADVANCED_FACE('',(#650),#467,.T.);
#4606=ADVANCED_FACE('',(#651),#468,.T.);
#4607=ADVANCED_FACE('',(#652),#469,.F.);
#4608=ADVANCED_FACE('',(#653),#470,.T.);
#4609=ADVANCED_FACE('',(#654),#471,.T.);
#4610=ADVANCED_FACE('',(#655),#472,.T.);
#4611=ADVANCED_FACE('',(#656),#473,.T.);
#4612=ADVANCED_FACE('',(#657),#474,.T.);
#4613=ADVANCED_FACE('',(#658),#475,.F.);
#4614=ADVANCED_FACE('',(#659,#366),#476,.T.);
#4615=ADVANCED_FACE('',(#660),#4501,.F.);
#4616=ADVANCED_FACE('',(#661,#367),#477,.T.);
#4617=ADVANCED_FACE('',(#662),#4502,.F.);
#4618=ADVANCED_FACE('',(#663,#368),#478,.T.);
#4619=ADVANCED_FACE('',(#664),#4503,.F.);
#4620=ADVANCED_FACE('',(#665,#369),#479,.T.);
#4621=ADVANCED_FACE('',(#666),#4504,.F.);
#4622=ADVANCED_FACE('',(#667,#370),#480,.T.);
#4623=ADVANCED_FACE('',(#668),#4505,.T.);
#4624=ADVANCED_FACE('',(#669),#4506,.T.);
#4625=ADVANCED_FACE('',(#670),#481,.T.);
#4626=ADVANCED_FACE('',(#671,#371),#482,.T.);
#4627=ADVANCED_FACE('',(#672),#483,.T.);
#4628=ADVANCED_FACE('',(#673),#484,.T.);
#4629=ADVANCED_FACE('',(#674),#485,.T.);
#4630=ADVANCED_FACE('',(#675),#486,.T.);
#4631=ADVANCED_FACE('',(#676),#487,.T.);
#4632=ADVANCED_FACE('',(#677),#488,.T.);
#4633=ADVANCED_FACE('',(#678),#489,.T.);
#4634=ADVANCED_FACE('',(#679),#490,.T.);
#4635=ADVANCED_FACE('',(#680),#491,.T.);
#4636=ADVANCED_FACE('',(#681),#492,.F.);
#4637=ADVANCED_FACE('',(#682,#372,#373),#4507,.T.);
#4638=ADVANCED_FACE('',(#683),#4508,.F.);
#4639=ADVANCED_FACE('',(#684),#493,.T.);
#4640=ADVANCED_FACE('',(#685),#494,.T.);
#4641=ADVANCED_FACE('',(#686),#495,.T.);
#4642=ADVANCED_FACE('',(#687),#496,.T.);
#4643=ADVANCED_FACE('',(#688,#374),#497,.F.);
#4644=ADVANCED_FACE('',(#689),#498,.T.);
#4645=ADVANCED_FACE('',(#690),#499,.T.);
#4646=ADVANCED_FACE('',(#691),#500,.T.);
#4647=ADVANCED_FACE('',(#692),#501,.T.);
#4648=ADVANCED_FACE('',(#693,#375),#502,.T.);
#4649=ADVANCED_FACE('',(#694),#503,.F.);
#4650=ADVANCED_FACE('',(#695),#4509,.F.);
#4651=ADVANCED_FACE('',(#696,#376),#504,.T.);
#4652=ADVANCED_FACE('',(#697),#505,.T.);
#4653=ADVANCED_FACE('',(#698),#506,.T.);
#4654=ADVANCED_FACE('',(#699),#507,.T.);
#4655=ADVANCED_FACE('',(#700),#508,.T.);
#4656=ADVANCED_FACE('',(#701,#377),#509,.F.);
#4657=ADVANCED_FACE('',(#702),#510,.T.);
#4658=ADVANCED_FACE('',(#703),#511,.T.);
#4659=ADVANCED_FACE('',(#704),#512,.T.);
#4660=ADVANCED_FACE('',(#705),#513,.T.);
#4661=ADVANCED_FACE('',(#706),#514,.T.);
#4662=ADVANCED_FACE('',(#707),#4510,.F.);
#4663=ADVANCED_FACE('',(#708),#4511,.F.);
#4664=ADVANCED_FACE('',(#709),#4512,.F.);
#4665=ADVANCED_FACE('',(#710),#4513,.F.);
#4666=ADVANCED_FACE('',(#711,#378),#515,.F.);
#4667=ADVANCED_FACE('',(#712),#4514,.T.);
#4668=ADVANCED_FACE('',(#713,#379),#516,.T.);
#4669=ADVANCED_FACE('',(#714),#4515,.T.);
#4670=ADVANCED_FACE('',(#715,#380,#381,#382,#383),#517,.F.);
#4671=ADVANCED_FACE('',(#716),#518,.T.);
#4672=ADVANCED_FACE('',(#717),#519,.T.);
#4673=ADVANCED_FACE('',(#718),#520,.T.);
#4674=ADVANCED_FACE('',(#719),#521,.T.);
#4675=ADVANCED_FACE('',(#720),#522,.T.);
#4676=ADVANCED_FACE('',(#721),#523,.F.);
#4677=ADVANCED_FACE('',(#722),#240,.T.);
#4678=ADVANCED_FACE('',(#723),#524,.T.);
#4679=ADVANCED_FACE('',(#724),#525,.F.);
#4680=ADVANCED_FACE('',(#725),#526,.F.);
#4681=ADVANCED_FACE('',(#726),#527,.F.);
#4682=ADVANCED_FACE('',(#727),#528,.F.);
#4683=ADVANCED_FACE('',(#728),#529,.F.);
#4684=ADVANCED_FACE('',(#729),#530,.F.);
#4685=ADVANCED_FACE('',(#730),#531,.F.);
#4686=ADVANCED_FACE('',(#731),#532,.F.);
#4687=ADVANCED_FACE('',(#732),#533,.F.);
#4688=ADVANCED_FACE('',(#733),#534,.F.);
#4689=ADVANCED_FACE('',(#734),#535,.T.);
#4690=ADVANCED_FACE('',(#735),#201,.T.);
#4691=ADVANCED_FACE('',(#736),#4516,.T.);
#4692=ADVANCED_FACE('',(#737),#202,.T.);
#4693=ADVANCED_FACE('',(#738,#384),#536,.T.);
#4694=ADVANCED_FACE('',(#739),#203,.T.);
#4695=ADVANCED_FACE('',(#740),#4517,.T.);
#4696=ADVANCED_FACE('',(#741),#4518,.F.);
#4697=ADVANCED_FACE('',(#742),#537,.T.);
#4698=ADVANCED_FACE('',(#743),#4519,.F.);
#4699=ADVANCED_FACE('',(#744),#538,.T.);
#4700=ADVANCED_FACE('',(#745),#4520,.F.);
#4701=ADVANCED_FACE('',(#746),#539,.T.);
#4702=ADVANCED_FACE('',(#747),#4521,.F.);
#4703=ADVANCED_FACE('',(#748),#540,.T.);
#4704=ADVANCED_FACE('',(#749),#4522,.F.);
#4705=ADVANCED_FACE('',(#750),#541,.F.);
#4706=ADVANCED_FACE('',(#751),#4523,.F.);
#4707=ADVANCED_FACE('',(#752),#542,.F.);
#4708=ADVANCED_FACE('',(#753),#4524,.F.);
#4709=ADVANCED_FACE('',(#754),#543,.F.);
#4710=ADVANCED_FACE('',(#755),#4525,.F.);
#4711=ADVANCED_FACE('',(#756),#544,.F.);
#4712=ADVANCED_FACE('',(#757),#4526,.F.);
#4713=ADVANCED_FACE('',(#758),#545,.F.);
#4714=ADVANCED_FACE('',(#759),#4527,.T.);
#4715=ADVANCED_FACE('',(#760,#385),#546,.F.);
#4716=ADVANCED_FACE('',(#761),#547,.T.);
#4717=ADVANCED_FACE('',(#762),#548,.T.);
#4718=ADVANCED_FACE('',(#763),#549,.T.);
#4719=ADVANCED_FACE('',(#764),#4528,.F.);
#4720=ADVANCED_FACE('',(#765,#386),#4529,.T.);
#4721=ADVANCED_FACE('',(#766,#387,#388,#389,#390,#391),#550,.T.);
#4722=ADVANCED_FACE('',(#767,#392,#393,#394,#395,#396),#551,.F.);
#4723=ADVANCED_FACE('',(#768),#4530,.F.);
#4724=ADVANCED_FACE('',(#769),#4531,.T.);
#4725=ADVANCED_FACE('',(#770,#397),#552,.T.);
#4726=ADVANCED_FACE('',(#771,#398),#553,.F.);
#4727=ADVANCED_FACE('',(#772),#4532,.F.);
#4728=ADVANCED_FACE('',(#773),#4533,.T.);
#4729=ADVANCED_FACE('',(#774,#399),#554,.T.);
#4730=ADVANCED_FACE('',(#775,#400),#555,.F.);
#4731=ADVANCED_FACE('',(#776),#4534,.F.);
#4732=ADVANCED_FACE('',(#777,#401),#556,.F.);
#4733=ADVANCED_FACE('',(#778),#4535,.F.);
#4734=ADVANCED_FACE('',(#779,#402),#557,.F.);
#4735=ADVANCED_FACE('',(#780),#4536,.F.);
#4736=ADVANCED_FACE('',(#781,#403),#558,.F.);
#4737=ADVANCED_FACE('',(#782),#4537,.F.);
#4738=ADVANCED_FACE('',(#783,#404),#559,.F.);
#4739=ADVANCED_FACE('',(#784),#4538,.F.);
#4740=ADVANCED_FACE('',(#785),#4539,.F.);
#4741=ADVANCED_FACE('',(#786),#4540,.F.);
#4742=ADVANCED_FACE('',(#787),#4541,.F.);
#4743=ADVANCED_FACE('',(#788),#4542,.T.);
#4744=ADVANCED_FACE('',(#789,#405),#560,.T.);
#4745=ADVANCED_FACE('',(#790),#4543,.F.);
#4746=ADVANCED_FACE('',(#791),#4544,.T.);
#4747=ADVANCED_FACE('',(#792,#406,#407,#408,#409,#410),#561,.T.);
#4748=ADVANCED_FACE('',(#793,#411,#412,#413,#414,#415),#562,.F.);
#4749=ADVANCED_FACE('',(#794),#4545,.F.);
#4750=ADVANCED_FACE('',(#795,#416),#563,.T.);
#4751=ADVANCED_FACE('',(#796),#4546,.F.);
#4752=ADVANCED_FACE('',(#797,#417),#564,.T.);
#4753=ADVANCED_FACE('',(#798),#4547,.F.);
#4754=ADVANCED_FACE('',(#799,#418),#565,.T.);
#4755=ADVANCED_FACE('',(#800),#4548,.F.);
#4756=ADVANCED_FACE('',(#801,#419),#566,.T.);
#4757=ADVANCED_FACE('',(#802),#4549,.F.);
#4758=ADVANCED_FACE('',(#803),#4550,.F.);
#4759=ADVANCED_FACE('',(#804),#4551,.F.);
#4760=ADVANCED_FACE('',(#805),#4552,.F.);
#4761=ADVANCED_FACE('',(#806),#567,.T.);
#4762=ADVANCED_FACE('',(#807),#568,.T.);
#4763=ADVANCED_FACE('',(#808),#569,.T.);
#4764=ADVANCED_FACE('',(#809),#4553,.T.);
#4765=ADVANCED_FACE('',(#810,#420),#570,.F.);
#4766=ADVANCED_FACE('',(#811),#4554,.F.);
#4767=ADVANCED_FACE('',(#812),#4555,.T.);
#4768=ADVANCED_FACE('',(#813,#421,#422,#423,#424,#425),#571,.T.);
#4769=ADVANCED_FACE('',(#814,#426,#427,#428,#429,#430),#572,.F.);
#4770=ADVANCED_FACE('',(#815),#4556,.T.);
#4771=ADVANCED_FACE('',(#816),#573,.T.);
#4772=ADVANCED_FACE('',(#817),#4557,.T.);
#4773=ADVANCED_FACE('',(#818,#431),#574,.T.);
#4774=ADVANCED_FACE('',(#819),#575,.F.);
#4775=ADVANCED_FACE('',(#820),#4558,.T.);
#4776=ADVANCED_FACE('',(#821),#576,.T.);
#4777=ADVANCED_FACE('',(#822),#577,.F.);
#4778=ADVANCED_FACE('',(#823),#27,.F.);
#4779=ADVANCED_FACE('',(#824),#4559,.T.);
#4780=ADVANCED_FACE('',(#825),#4560,.F.);
#4781=ADVANCED_FACE('',(#826),#204,.F.);
#4782=ADVANCED_FACE('',(#827,#432),#578,.T.);
#4783=ADVANCED_FACE('',(#828),#4561,.T.);
#4784=ADVANCED_FACE('',(#829,#433),#579,.T.);
#4785=ADVANCED_FACE('',(#830),#205,.F.);
#4786=ADVANCED_FACE('',(#831),#28,.F.);
#4787=ADVANCED_FACE('',(#832),#4562,.F.);
#4788=ADVANCED_FACE('',(#833,#434),#580,.T.);
#4789=ADVANCED_FACE('',(#834),#206,.T.);
#4790=ADVANCED_FACE('',(#835),#4563,.T.);
#4791=ADVANCED_FACE('',(#836),#207,.T.);
#4792=ADVANCED_FACE('',(#837,#435),#581,.T.);
#4793=ADVANCED_FACE('',(#838),#4564,.F.);
#4794=ADVANCED_FACE('',(#839),#11,.T.);
#4795=ADVANCED_FACE('',(#840),#12,.T.);
#4796=ADVANCED_FACE('',(#841),#13,.T.);
#4797=ADVANCED_FACE('',(#842),#14,.T.);
#4798=ADVANCED_FACE('',(#843),#15,.T.);
#4799=ADVANCED_FACE('',(#844),#16,.T.);
#4800=ADVANCED_FACE('',(#845),#17,.T.);
#4801=ADVANCED_FACE('',(#846),#18,.T.);
#4802=ADVANCED_FACE('',(#847),#19,.F.);
#4803=ADVANCED_FACE('',(#848),#4565,.T.);
#4804=ADVANCED_FACE('',(#849),#582,.T.);
#4805=ADVANCED_FACE('',(#850),#20,.F.);
#4806=ADVANCED_FACE('',(#851),#583,.T.);
#4807=ADVANCED_FACE('',(#852),#21,.F.);
#4808=ADVANCED_FACE('',(#853),#584,.T.);
#4809=ADVANCED_FACE('',(#854),#22,.F.);
#4810=ADVANCED_FACE('',(#855),#585,.T.);
#4811=ADVANCED_FACE('',(#856),#23,.F.);
#4812=ADVANCED_FACE('',(#857),#586,.T.);
#4813=ADVANCED_FACE('',(#858),#24,.F.);
#4814=ADVANCED_FACE('',(#859),#587,.T.);
#4815=ADVANCED_FACE('',(#860),#25,.F.);
#4816=ADVANCED_FACE('',(#861),#4566,.F.);
#4817=ADVANCED_FACE('',(#862),#588,.T.);
#4818=ADVANCED_FACE('',(#863),#26,.F.);
#4819=ADVANCED_FACE('',(#864,#436),#589,.T.);
#4820=ADVANCED_FACE('',(#865),#590,.T.);
#4821=ADVANCED_FACE('',(#866,#437),#591,.T.);
#4822=ADVANCED_FACE('',(#867),#4567,.T.);
#4823=ADVANCED_FACE('',(#868,#438),#592,.T.);
#4824=ADVANCED_FACE('',(#869),#4568,.F.);
#4825=ADVANCED_FACE('',(#870,#439),#593,.T.);
#4826=ADVANCED_FACE('',(#871),#4569,.T.);
#4827=ADVANCED_FACE('',(#872,#440),#594,.T.);
#4828=ADVANCED_FACE('',(#873),#4570,.F.);
#4829=ADVANCED_FACE('',(#874),#4571,.F.);
#4830=ADVANCED_FACE('',(#875),#595,.T.);
#4831=ADVANCED_FACE('',(#876),#4572,.F.);
#4832=ADVANCED_FACE('',(#877),#596,.F.);
#4833=ADVANCED_FACE('',(#878,#441),#597,.T.);
#4834=ADVANCED_FACE('',(#879),#4573,.T.);
#4835=ADVANCED_FACE('',(#880,#442),#598,.F.);
#4836=ADVANCED_FACE('',(#881),#4574,.T.);
#4837=ADVANCED_FACE('',(#882),#4575,.T.);
#4838=ADVANCED_FACE('',(#883),#4576,.T.);
#4839=ADVANCED_FACE('',(#884,#443),#599,.T.);
#4840=ADVANCED_FACE('',(#885,#444),#600,.F.);
#4841=ADVANCED_FACE('',(#886),#4577,.T.);
#4842=ADVANCED_FACE('',(#887,#445),#601,.T.);
#4843=ADVANCED_FACE('',(#888,#446),#602,.F.);
#4844=ADVANCED_FACE('',(#889),#4578,.F.);
#4845=ADVANCED_FACE('',(#890),#4579,.T.);
#4846=ADVANCED_FACE('',(#891,#447,#448),#603,.F.);
#4847=ADVANCED_FACE('',(#892),#604,.T.);
#4848=ADVANCED_FACE('',(#893),#605,.T.);
#4849=ADVANCED_FACE('',(#894,#449),#606,.T.);
#4850=ADVANCED_FACE('',(#895),#4580,.F.);
#4851=ADVANCED_FACE('',(#896),#4581,.T.);
#4852=ADVANCED_FACE('',(#897,#450),#607,.T.);
#4853=ADVANCED_FACE('',(#898),#4582,.F.);
#4854=ADVANCED_FACE('',(#899),#608,.T.);
#4855=ADVANCED_FACE('',(#900),#4583,.T.);
#4856=ADVANCED_FACE('',(#901,#451),#609,.T.);
#4857=ADVANCED_FACE('',(#902),#610,.F.);
#4858=ADVANCED_FACE('',(#903),#4584,.F.);
#4859=ADVANCED_FACE('',(#904),#4585,.T.);
#4860=ADVANCED_FACE('',(#905,#452),#611,.T.);
#4861=ADVANCED_FACE('',(#906,#453),#612,.F.);
#4862=ADVANCED_FACE('',(#907),#4586,.F.);
#4863=ADVANCED_FACE('',(#908),#4587,.T.);
#4864=ADVANCED_FACE('',(#909,#454),#613,.T.);
#4865=ADVANCED_FACE('',(#910,#455),#614,.F.);
#4866=ADVANCED_FACE('',(#911),#615,.T.);
#4867=ADVANCED_FACE('',(#912),#208,.T.);
#4868=ADVANCED_FACE('',(#913),#4588,.T.);
#4869=ADVANCED_FACE('',(#914),#209,.T.);
#4870=ADVANCED_FACE('',(#915,#456),#616,.T.);
#4871=ADVANCED_FACE('',(#916),#210,.T.);
#4872=ADVANCED_FACE('',(#917),#4589,.T.);
#4873=ADVANCED_FACE('',(#918),#211,.T.);
#4874=ADVANCED_FACE('',(#919),#617,.T.);
#4875=ADVANCED_FACE('',(#920),#618,.F.);
#4876=ADVANCED_FACE('',(#921),#619,.F.);
#4877=ADVANCED_FACE('',(#922),#620,.F.);
#4878=ADVANCED_FACE('',(#923),#621,.F.);
#4879=ADVANCED_FACE('',(#924),#622,.F.);
#4880=ADVANCED_FACE('',(#925),#623,.F.);
#4881=ADVANCED_FACE('',(#926),#624,.F.);
#4882=ADVANCED_FACE('',(#927),#625,.F.);
#4883=ADVANCED_FACE('',(#928),#626,.F.);
#4884=ADVANCED_FACE('',(#929),#627,.F.);
#4885=ADVANCED_FACE('',(#930),#628,.F.);
#4886=ADVANCED_FACE('',(#931),#629,.F.);
#4887=ADVANCED_FACE('',(#932),#630,.F.);
#4888=ADVANCED_FACE('',(#933),#631,.F.);
#4889=ADVANCED_FACE('',(#934),#632,.F.);
#4890=ADVANCED_FACE('',(#935),#633,.F.);
#4891=ADVANCED_FACE('',(#936),#634,.F.);
#4892=ADVANCED_FACE('',(#937),#635,.T.);
#4893=ADVANCED_FACE('',(#938),#212,.T.);
#4894=ADVANCED_FACE('',(#939),#4590,.T.);
#4895=ADVANCED_FACE('',(#940),#213,.T.);
#4896=ADVANCED_FACE('',(#941,#457),#636,.T.);
#4897=ADVANCED_FACE('',(#942),#214,.T.);
#4898=ADVANCED_FACE('',(#943),#4591,.T.);
#4899=CLOSED_SHELL('',(#4592,#4593,#4594,#4595,#4596,#4597,#4598,#4599,
#4600,#4601));
#4900=CLOSED_SHELL('',(#4602,#4603,#4604,#4605,#4606,#4607));
#4901=CLOSED_SHELL('',(#4608,#4609,#4610,#4611,#4612,#4613));
#4902=CLOSED_SHELL('',(#4614,#4615,#4616,#4617,#4618,#4619,#4620,#4621,
#4622,#4623,#4624,#4625,#4626,#4627,#4628,#4629,#4630,#4631,#4632,#4633,
#4634,#4635,#4636,#4637,#4638,#4639,#4640,#4641,#4642,#4643,#4644,#4645,
#4646,#4647,#4648,#4649,#4650,#4651,#4652,#4653,#4654,#4655,#4656,#4657,
#4658,#4659,#4660,#4661,#4662,#4663,#4664,#4665,#4666,#4667,#4668,#4669,
#4670));
#4903=CLOSED_SHELL('',(#4671,#4672,#4673,#4674,#4675,#4676));
#4904=CLOSED_SHELL('',(#4677,#4678,#4679));
#4905=CLOSED_SHELL('',(#4680,#4681,#4682,#4683,#4684,#4685,#4686,#4687));
#4906=CLOSED_SHELL('',(#4688,#4689,#4690,#4691,#4692,#4693,#4694,#4695));
#4907=CLOSED_SHELL('',(#4696,#4697,#4698,#4699,#4700,#4701,#4702,#4703,
#4704,#4705,#4706,#4707,#4708,#4709,#4710,#4711,#4712,#4713,#4714,#4715,
#4716,#4717,#4718,#4719,#4720,#4721,#4722));
#4908=CLOSED_SHELL('',(#4723,#4724,#4725,#4726));
#4909=CLOSED_SHELL('',(#4727,#4728,#4729,#4730));
#4910=CLOSED_SHELL('',(#4731,#4732,#4733,#4734,#4735,#4736,#4737,#4738,
#4739,#4740,#4741,#4742,#4743,#4744,#4745,#4746,#4747,#4748));
#4911=CLOSED_SHELL('',(#4749,#4750,#4751,#4752,#4753,#4754,#4755,#4756,
#4757,#4758,#4759,#4760,#4761,#4762,#4763,#4764,#4765,#4766,#4767,#4768,
#4769));
#4912=CLOSED_SHELL('',(#4770,#4771,#4772,#4773,#4774));
#4913=CLOSED_SHELL('',(#4775,#4776,#4777));
#4914=CLOSED_SHELL('',(#4778,#4779,#4780,#4781,#4782,#4783,#4784,#4785));
#4915=CLOSED_SHELL('',(#4786,#4787,#4788,#4789,#4790,#4791,#4792,#4793));
#4916=CLOSED_SHELL('',(#4794));
#4917=CLOSED_SHELL('',(#4795));
#4918=CLOSED_SHELL('',(#4796));
#4919=CLOSED_SHELL('',(#4797));
#4920=CLOSED_SHELL('',(#4798));
#4921=CLOSED_SHELL('',(#4799));
#4922=CLOSED_SHELL('',(#4800));
#4923=CLOSED_SHELL('',(#4801));
#4924=CLOSED_SHELL('',(#4802,#4803,#4804,#4805,#4806,#4807,#4808,#4809,
#4810,#4811,#4812,#4813,#4814,#4815,#4816,#4817,#4818,#4819,#4820));
#4925=CLOSED_SHELL('',(#4821,#4822,#4823,#4824));
#4926=CLOSED_SHELL('',(#4825,#4826,#4827,#4828));
#4927=CLOSED_SHELL('',(#4829,#4830,#4831,#4832,#4833,#4834,#4835,#4836,
#4837,#4838,#4839,#4840,#4841,#4842,#4843));
#4928=CLOSED_SHELL('',(#4844,#4845,#4846,#4847,#4848,#4849,#4850,#4851,
#4852));
#4929=CLOSED_SHELL('',(#4853,#4854,#4855,#4856,#4857));
#4930=CLOSED_SHELL('',(#4858,#4859,#4860,#4861));
#4931=CLOSED_SHELL('',(#4862,#4863,#4864,#4865));
#4932=CLOSED_SHELL('',(#4866,#4867,#4868,#4869,#4870,#4871,#4872,#4873,
#4874));
#4933=CLOSED_SHELL('',(#4875,#4876,#4877,#4878,#4879,#4880,#4881,#4882));
#4934=CLOSED_SHELL('',(#4883,#4884,#4885,#4886,#4887,#4888,#4889,#4890));
#4935=CLOSED_SHELL('',(#4891,#4892,#4893,#4894,#4895,#4896,#4897,#4898));
#4936=DERIVED_UNIT_ELEMENT(#4988,1.);
#4937=DERIVED_UNIT_ELEMENT(#10629,-3.);
#4938=DERIVED_UNIT_ELEMENT(#4988,1.);
#4939=DERIVED_UNIT_ELEMENT(#10629,-3.);
#4940=DERIVED_UNIT_ELEMENT(#4988,1.);
#4941=DERIVED_UNIT_ELEMENT(#10629,-3.);
#4942=DERIVED_UNIT_ELEMENT(#4988,1.);
#4943=DERIVED_UNIT_ELEMENT(#10629,-3.);
#4944=DERIVED_UNIT_ELEMENT(#4988,1.);
#4945=DERIVED_UNIT_ELEMENT(#10629,-3.);
#4946=DERIVED_UNIT_ELEMENT(#4988,1.);
#4947=DERIVED_UNIT_ELEMENT(#10629,-3.);
#4948=DERIVED_UNIT_ELEMENT(#4988,1.);
#4949=DERIVED_UNIT_ELEMENT(#10629,-3.);
#4950=DERIVED_UNIT_ELEMENT(#4988,1.);
#4951=DERIVED_UNIT_ELEMENT(#10629,-3.);
#4952=DERIVED_UNIT_ELEMENT(#4988,1.);
#4953=DERIVED_UNIT_ELEMENT(#10629,-3.);
#4954=DERIVED_UNIT_ELEMENT(#4988,1.);
#4955=DERIVED_UNIT_ELEMENT(#10629,-3.);
#4956=DERIVED_UNIT_ELEMENT(#4988,1.);
#4957=DERIVED_UNIT_ELEMENT(#10629,-3.);
#4958=DERIVED_UNIT_ELEMENT(#4988,1.);
#4959=DERIVED_UNIT_ELEMENT(#10629,-3.);
#4960=DERIVED_UNIT_ELEMENT(#4988,1.);
#4961=DERIVED_UNIT_ELEMENT(#10629,-3.);
#4962=DERIVED_UNIT_ELEMENT(#4988,1.);
#4963=DERIVED_UNIT_ELEMENT(#10629,-3.);
#4964=DERIVED_UNIT_ELEMENT(#4988,1.);
#4965=DERIVED_UNIT_ELEMENT(#10629,-3.);
#4966=DERIVED_UNIT_ELEMENT(#4988,1.);
#4967=DERIVED_UNIT_ELEMENT(#10629,-3.);
#4968=DERIVED_UNIT_ELEMENT(#4988,1.);
#4969=DERIVED_UNIT_ELEMENT(#10629,-3.);
#4970=DERIVED_UNIT_ELEMENT(#4988,1.);
#4971=DERIVED_UNIT_ELEMENT(#10629,-3.);
#4972=DERIVED_UNIT_ELEMENT(#4988,1.);
#4973=DERIVED_UNIT_ELEMENT(#10629,-3.);
#4974=DERIVED_UNIT_ELEMENT(#4988,1.);
#4975=DERIVED_UNIT_ELEMENT(#10629,-3.);
#4976=DERIVED_UNIT_ELEMENT(#4988,1.);
#4977=DERIVED_UNIT_ELEMENT(#10629,-3.);
#4978=DERIVED_UNIT_ELEMENT(#4988,1.);
#4979=DERIVED_UNIT_ELEMENT(#10629,-3.);
#4980=DERIVED_UNIT_ELEMENT(#4988,1.);
#4981=DERIVED_UNIT_ELEMENT(#10629,-3.);
#4982=DERIVED_UNIT_ELEMENT(#4988,1.);
#4983=DERIVED_UNIT_ELEMENT(#10629,-3.);
#4984=DERIVED_UNIT_ELEMENT(#4988,1.);
#4985=DERIVED_UNIT_ELEMENT(#10629,-3.);
#4986=DERIVED_UNIT_ELEMENT(#4988,1.);
#4987=DERIVED_UNIT_ELEMENT(#10629,-3.);
#4988=(
MASS_UNIT()
NAMED_UNIT(*)
SI_UNIT(.KILO.,.GRAM.)
);
#4989=DERIVED_UNIT((#4936,#4937));
#4990=DERIVED_UNIT((#4938,#4939));
#4991=DERIVED_UNIT((#4940,#4941));
#4992=DERIVED_UNIT((#4942,#4943));
#4993=DERIVED_UNIT((#4944,#4945));
#4994=DERIVED_UNIT((#4946,#4947));
#4995=DERIVED_UNIT((#4948,#4949));
#4996=DERIVED_UNIT((#4950,#4951));
#4997=DERIVED_UNIT((#4952,#4953));
#4998=DERIVED_UNIT((#4954,#4955));
#4999=DERIVED_UNIT((#4956,#4957));
#5000=DERIVED_UNIT((#4958,#4959));
#5001=DERIVED_UNIT((#4960,#4961));
#5002=DERIVED_UNIT((#4962,#4963));
#5003=DERIVED_UNIT((#4964,#4965));
#5004=DERIVED_UNIT((#4966,#4967));
#5005=DERIVED_UNIT((#4968,#4969));
#5006=DERIVED_UNIT((#4970,#4971));
#5007=DERIVED_UNIT((#4972,#4973));
#5008=DERIVED_UNIT((#4974,#4975));
#5009=DERIVED_UNIT((#4976,#4977));
#5010=DERIVED_UNIT((#4978,#4979));
#5011=DERIVED_UNIT((#4980,#4981));
#5012=DERIVED_UNIT((#4982,#4983));
#5013=DERIVED_UNIT((#4984,#4985));
#5014=DERIVED_UNIT((#4986,#4987));
#5015=MEASURE_REPRESENTATION_ITEM('density measure',
POSITIVE_RATIO_MEASURE(7850.),#4989);
#5016=MEASURE_REPRESENTATION_ITEM('density measure',
POSITIVE_RATIO_MEASURE(7850.),#4990);
#5017=MEASURE_REPRESENTATION_ITEM('density measure',
POSITIVE_RATIO_MEASURE(7850.),#4991);
#5018=MEASURE_REPRESENTATION_ITEM('density measure',
POSITIVE_RATIO_MEASURE(7850.),#4992);
#5019=MEASURE_REPRESENTATION_ITEM('density measure',
POSITIVE_RATIO_MEASURE(7850.),#4993);
#5020=MEASURE_REPRESENTATION_ITEM('density measure',
POSITIVE_RATIO_MEASURE(7850.),#4994);
#5021=MEASURE_REPRESENTATION_ITEM('density measure',
POSITIVE_RATIO_MEASURE(7850.),#4995);
#5022=MEASURE_REPRESENTATION_ITEM('density measure',
POSITIVE_RATIO_MEASURE(7850.),#4996);
#5023=MEASURE_REPRESENTATION_ITEM('density measure',
POSITIVE_RATIO_MEASURE(7850.),#4997);
#5024=MEASURE_REPRESENTATION_ITEM('density measure',
POSITIVE_RATIO_MEASURE(7850.),#4998);
#5025=MEASURE_REPRESENTATION_ITEM('density measure',
POSITIVE_RATIO_MEASURE(7850.),#4999);
#5026=MEASURE_REPRESENTATION_ITEM('density measure',
POSITIVE_RATIO_MEASURE(7850.),#5000);
#5027=MEASURE_REPRESENTATION_ITEM('density measure',
POSITIVE_RATIO_MEASURE(7850.),#5001);
#5028=MEASURE_REPRESENTATION_ITEM('density measure',
POSITIVE_RATIO_MEASURE(7850.),#5002);
#5029=MEASURE_REPRESENTATION_ITEM('density measure',
POSITIVE_RATIO_MEASURE(7850.),#5003);
#5030=MEASURE_REPRESENTATION_ITEM('density measure',
POSITIVE_RATIO_MEASURE(7850.),#5004);
#5031=MEASURE_REPRESENTATION_ITEM('density measure',
POSITIVE_RATIO_MEASURE(7850.),#5005);
#5032=MEASURE_REPRESENTATION_ITEM('density measure',
POSITIVE_RATIO_MEASURE(7850.),#5006);
#5033=MEASURE_REPRESENTATION_ITEM('density measure',
POSITIVE_RATIO_MEASURE(7850.),#5007);
#5034=MEASURE_REPRESENTATION_ITEM('density measure',
POSITIVE_RATIO_MEASURE(7850.),#5008);
#5035=MEASURE_REPRESENTATION_ITEM('density measure',
POSITIVE_RATIO_MEASURE(7850.),#5009);
#5036=MEASURE_REPRESENTATION_ITEM('density measure',
POSITIVE_RATIO_MEASURE(7850.),#5010);
#5037=MEASURE_REPRESENTATION_ITEM('density measure',
POSITIVE_RATIO_MEASURE(7850.),#5011);
#5038=MEASURE_REPRESENTATION_ITEM('density measure',
POSITIVE_RATIO_MEASURE(7850.),#5012);
#5039=MEASURE_REPRESENTATION_ITEM('density measure',
POSITIVE_RATIO_MEASURE(7850.),#5013);
#5040=MEASURE_REPRESENTATION_ITEM('density measure',
POSITIVE_RATIO_MEASURE(7850.),#5014);
#5041=PROPERTY_DEFINITION_REPRESENTATION(#5171,#5093);
#5042=PROPERTY_DEFINITION_REPRESENTATION(#5172,#5094);
#5043=PROPERTY_DEFINITION_REPRESENTATION(#5173,#5095);
#5044=PROPERTY_DEFINITION_REPRESENTATION(#5174,#5096);
#5045=PROPERTY_DEFINITION_REPRESENTATION(#5175,#5097);
#5046=PROPERTY_DEFINITION_REPRESENTATION(#5176,#5098);
#5047=PROPERTY_DEFINITION_REPRESENTATION(#5177,#5099);
#5048=PROPERTY_DEFINITION_REPRESENTATION(#5178,#5100);
#5049=PROPERTY_DEFINITION_REPRESENTATION(#5179,#5101);
#5050=PROPERTY_DEFINITION_REPRESENTATION(#5180,#5102);
#5051=PROPERTY_DEFINITION_REPRESENTATION(#5181,#5103);
#5052=PROPERTY_DEFINITION_REPRESENTATION(#5182,#5104);
#5053=PROPERTY_DEFINITION_REPRESENTATION(#5183,#5105);
#5054=PROPERTY_DEFINITION_REPRESENTATION(#5184,#5106);
#5055=PROPERTY_DEFINITION_REPRESENTATION(#5185,#5107);
#5056=PROPERTY_DEFINITION_REPRESENTATION(#5186,#5108);
#5057=PROPERTY_DEFINITION_REPRESENTATION(#5187,#5109);
#5058=PROPERTY_DEFINITION_REPRESENTATION(#5188,#5110);
#5059=PROPERTY_DEFINITION_REPRESENTATION(#5189,#5111);
#5060=PROPERTY_DEFINITION_REPRESENTATION(#5190,#5112);
#5061=PROPERTY_DEFINITION_REPRESENTATION(#5191,#5113);
#5062=PROPERTY_DEFINITION_REPRESENTATION(#5192,#5114);
#5063=PROPERTY_DEFINITION_REPRESENTATION(#5193,#5115);
#5064=PROPERTY_DEFINITION_REPRESENTATION(#5194,#5116);
#5065=PROPERTY_DEFINITION_REPRESENTATION(#5195,#5117);
#5066=PROPERTY_DEFINITION_REPRESENTATION(#5196,#5118);
#5067=PROPERTY_DEFINITION_REPRESENTATION(#5197,#5119);
#5068=PROPERTY_DEFINITION_REPRESENTATION(#5198,#5120);
#5069=PROPERTY_DEFINITION_REPRESENTATION(#5199,#5121);
#5070=PROPERTY_DEFINITION_REPRESENTATION(#5200,#5122);
#5071=PROPERTY_DEFINITION_REPRESENTATION(#5201,#5123);
#5072=PROPERTY_DEFINITION_REPRESENTATION(#5202,#5124);
#5073=PROPERTY_DEFINITION_REPRESENTATION(#5203,#5125);
#5074=PROPERTY_DEFINITION_REPRESENTATION(#5204,#5126);
#5075=PROPERTY_DEFINITION_REPRESENTATION(#5205,#5127);
#5076=PROPERTY_DEFINITION_REPRESENTATION(#5206,#5128);
#5077=PROPERTY_DEFINITION_REPRESENTATION(#5207,#5129);
#5078=PROPERTY_DEFINITION_REPRESENTATION(#5208,#5130);
#5079=PROPERTY_DEFINITION_REPRESENTATION(#5209,#5131);
#5080=PROPERTY_DEFINITION_REPRESENTATION(#5210,#5132);
#5081=PROPERTY_DEFINITION_REPRESENTATION(#5211,#5133);
#5082=PROPERTY_DEFINITION_REPRESENTATION(#5212,#5134);
#5083=PROPERTY_DEFINITION_REPRESENTATION(#5213,#5135);
#5084=PROPERTY_DEFINITION_REPRESENTATION(#5214,#5136);
#5085=PROPERTY_DEFINITION_REPRESENTATION(#5215,#5137);
#5086=PROPERTY_DEFINITION_REPRESENTATION(#5216,#5138);
#5087=PROPERTY_DEFINITION_REPRESENTATION(#5217,#5139);
#5088=PROPERTY_DEFINITION_REPRESENTATION(#5218,#5140);
#5089=PROPERTY_DEFINITION_REPRESENTATION(#5219,#5141);
#5090=PROPERTY_DEFINITION_REPRESENTATION(#5220,#5142);
#5091=PROPERTY_DEFINITION_REPRESENTATION(#5221,#5143);
#5092=PROPERTY_DEFINITION_REPRESENTATION(#5222,#5144);
#5093=REPRESENTATION('material name',(#5145),#10598);
#5094=REPRESENTATION('density',(#5015),#10598);
#5095=REPRESENTATION('material name',(#5146),#10599);
#5096=REPRESENTATION('density',(#5016),#10599);
#5097=REPRESENTATION('material name',(#5147),#10600);
#5098=REPRESENTATION('density',(#5017),#10600);
#5099=REPRESENTATION('material name',(#5148),#10601);
#5100=REPRESENTATION('density',(#5018),#10601);
#5101=REPRESENTATION('material name',(#5149),#10602);
#5102=REPRESENTATION('density',(#5019),#10602);
#5103=REPRESENTATION('material name',(#5150),#10603);
#5104=REPRESENTATION('density',(#5020),#10603);
#5105=REPRESENTATION('material name',(#5151),#10604);
#5106=REPRESENTATION('density',(#5021),#10604);
#5107=REPRESENTATION('material name',(#5152),#10606);
#5108=REPRESENTATION('density',(#5022),#10606);
#5109=REPRESENTATION('material name',(#5153),#10607);
#5110=REPRESENTATION('density',(#5023),#10607);
#5111=REPRESENTATION('material name',(#5154),#10608);
#5112=REPRESENTATION('density',(#5024),#10608);
#5113=REPRESENTATION('material name',(#5155),#10609);
#5114=REPRESENTATION('density',(#5025),#10609);
#5115=REPRESENTATION('material name',(#5156),#10610);
#5116=REPRESENTATION('density',(#5026),#10610);
#5117=REPRESENTATION('material name',(#5157),#10611);
#5118=REPRESENTATION('density',(#5027),#10611);
#5119=REPRESENTATION('material name',(#5158),#10612);
#5120=REPRESENTATION('density',(#5028),#10612);
#5121=REPRESENTATION('material name',(#5159),#10614);
#5122=REPRESENTATION('density',(#5029),#10614);
#5123=REPRESENTATION('material name',(#5160),#10615);
#5124=REPRESENTATION('density',(#5030),#10615);
#5125=REPRESENTATION('material name',(#5161),#10616);
#5126=REPRESENTATION('density',(#5031),#10616);
#5127=REPRESENTATION('material name',(#5162),#10617);
#5128=REPRESENTATION('density',(#5032),#10617);
#5129=REPRESENTATION('material name',(#5163),#10618);
#5130=REPRESENTATION('density',(#5033),#10618);
#5131=REPRESENTATION('material name',(#5164),#10620);
#5132=REPRESENTATION('density',(#5034),#10620);
#5133=REPRESENTATION('material name',(#5165),#10621);
#5134=REPRESENTATION('density',(#5035),#10621);
#5135=REPRESENTATION('material name',(#5166),#10622);
#5136=REPRESENTATION('density',(#5036),#10622);
#5137=REPRESENTATION('material name',(#5167),#10623);
#5138=REPRESENTATION('density',(#5037),#10623);
#5139=REPRESENTATION('material name',(#5168),#10624);
#5140=REPRESENTATION('density',(#5038),#10624);
#5141=REPRESENTATION('material name',(#5169),#10625);
#5142=REPRESENTATION('density',(#5039),#10625);
#5143=REPRESENTATION('material name',(#5170),#10626);
#5144=REPRESENTATION('density',(#5040),#10626);
#5145=DESCRIPTIVE_REPRESENTATION_ITEM('Steel','Steel');
#5146=DESCRIPTIVE_REPRESENTATION_ITEM('Steel','Steel');
#5147=DESCRIPTIVE_REPRESENTATION_ITEM('Steel','Steel');
#5148=DESCRIPTIVE_REPRESENTATION_ITEM('Steel','Steel');
#5149=DESCRIPTIVE_REPRESENTATION_ITEM('Steel','Steel');
#5150=DESCRIPTIVE_REPRESENTATION_ITEM('Steel','Steel');
#5151=DESCRIPTIVE_REPRESENTATION_ITEM('Steel','Steel');
#5152=DESCRIPTIVE_REPRESENTATION_ITEM('Steel','Steel');
#5153=DESCRIPTIVE_REPRESENTATION_ITEM('Steel','Steel');
#5154=DESCRIPTIVE_REPRESENTATION_ITEM('Steel','Steel');
#5155=DESCRIPTIVE_REPRESENTATION_ITEM('Steel','Steel');
#5156=DESCRIPTIVE_REPRESENTATION_ITEM('Steel','Steel');
#5157=DESCRIPTIVE_REPRESENTATION_ITEM('Steel','Steel');
#5158=DESCRIPTIVE_REPRESENTATION_ITEM('Steel','Steel');
#5159=DESCRIPTIVE_REPRESENTATION_ITEM('Steel','Steel');
#5160=DESCRIPTIVE_REPRESENTATION_ITEM('Steel','Steel');
#5161=DESCRIPTIVE_REPRESENTATION_ITEM('Steel','Steel');
#5162=DESCRIPTIVE_REPRESENTATION_ITEM('Steel','Steel');
#5163=DESCRIPTIVE_REPRESENTATION_ITEM('Steel','Steel');
#5164=DESCRIPTIVE_REPRESENTATION_ITEM('Steel','Steel');
#5165=DESCRIPTIVE_REPRESENTATION_ITEM('Steel','Steel');
#5166=DESCRIPTIVE_REPRESENTATION_ITEM('Steel','Steel');
#5167=DESCRIPTIVE_REPRESENTATION_ITEM('Steel','Steel');
#5168=DESCRIPTIVE_REPRESENTATION_ITEM('Steel','Steel');
#5169=DESCRIPTIVE_REPRESENTATION_ITEM('Steel','Steel');
#5170=DESCRIPTIVE_REPRESENTATION_ITEM('Steel','Steel');
#5171=PROPERTY_DEFINITION('material property','material name',#10771);
#5172=PROPERTY_DEFINITION('material property','density of part',#10771);
#5173=PROPERTY_DEFINITION('material property','material name',#10772);
#5174=PROPERTY_DEFINITION('material property','density of part',#10772);
#5175=PROPERTY_DEFINITION('material property','material name',#10773);
#5176=PROPERTY_DEFINITION('material property','density of part',#10773);
#5177=PROPERTY_DEFINITION('material property','material name',#10774);
#5178=PROPERTY_DEFINITION('material property','density of part',#10774);
#5179=PROPERTY_DEFINITION('material property','material name',#10775);
#5180=PROPERTY_DEFINITION('material property','density of part',#10775);
#5181=PROPERTY_DEFINITION('material property','material name',#10776);
#5182=PROPERTY_DEFINITION('material property','density of part',#10776);
#5183=PROPERTY_DEFINITION('material property','material name',#10777);
#5184=PROPERTY_DEFINITION('material property','density of part',#10777);
#5185=PROPERTY_DEFINITION('material property','material name',#10779);
#5186=PROPERTY_DEFINITION('material property','density of part',#10779);
#5187=PROPERTY_DEFINITION('material property','material name',#10780);
#5188=PROPERTY_DEFINITION('material property','density of part',#10780);
#5189=PROPERTY_DEFINITION('material property','material name',#10781);
#5190=PROPERTY_DEFINITION('material property','density of part',#10781);
#5191=PROPERTY_DEFINITION('material property','material name',#10782);
#5192=PROPERTY_DEFINITION('material property','density of part',#10782);
#5193=PROPERTY_DEFINITION('material property','material name',#10783);
#5194=PROPERTY_DEFINITION('material property','density of part',#10783);
#5195=PROPERTY_DEFINITION('material property','material name',#10784);
#5196=PROPERTY_DEFINITION('material property','density of part',#10784);
#5197=PROPERTY_DEFINITION('material property','material name',#10785);
#5198=PROPERTY_DEFINITION('material property','density of part',#10785);
#5199=PROPERTY_DEFINITION('material property','material name',#10787);
#5200=PROPERTY_DEFINITION('material property','density of part',#10787);
#5201=PROPERTY_DEFINITION('material property','material name',#10788);
#5202=PROPERTY_DEFINITION('material property','density of part',#10788);
#5203=PROPERTY_DEFINITION('material property','material name',#10789);
#5204=PROPERTY_DEFINITION('material property','density of part',#10789);
#5205=PROPERTY_DEFINITION('material property','material name',#10790);
#5206=PROPERTY_DEFINITION('material property','density of part',#10790);
#5207=PROPERTY_DEFINITION('material property','material name',#10791);
#5208=PROPERTY_DEFINITION('material property','density of part',#10791);
#5209=PROPERTY_DEFINITION('material property','material name',#10793);
#5210=PROPERTY_DEFINITION('material property','density of part',#10793);
#5211=PROPERTY_DEFINITION('material property','material name',#10794);
#5212=PROPERTY_DEFINITION('material property','density of part',#10794);
#5213=PROPERTY_DEFINITION('material property','material name',#10795);
#5214=PROPERTY_DEFINITION('material property','density of part',#10795);
#5215=PROPERTY_DEFINITION('material property','material name',#10796);
#5216=PROPERTY_DEFINITION('material property','density of part',#10796);
#5217=PROPERTY_DEFINITION('material property','material name',#10797);
#5218=PROPERTY_DEFINITION('material property','density of part',#10797);
#5219=PROPERTY_DEFINITION('material property','material name',#10798);
#5220=PROPERTY_DEFINITION('material property','density of part',#10798);
#5221=PROPERTY_DEFINITION('material property','material name',#10799);
#5222=PROPERTY_DEFINITION('material property','density of part',#10799);
#5223=AXIS2_PLACEMENT_3D('',#7486,#5870,#5871);
#5224=AXIS2_PLACEMENT_3D('',#7487,#5872,#5873);
#5225=AXIS2_PLACEMENT_3D('',#7488,#5874,#5875);
#5226=AXIS2_PLACEMENT_3D('',#7489,#5876,#5877);
#5227=AXIS2_PLACEMENT_3D('',#7491,#5878,#5879);
#5228=AXIS2_PLACEMENT_3D('',#7494,#5881,#5882);
#5229=AXIS2_PLACEMENT_3D('',#7495,#5883,#5884);
#5230=AXIS2_PLACEMENT_3D('',#7497,#5885,#5886);
#5231=AXIS2_PLACEMENT_3D('',#7500,#5888,#5889);
#5232=AXIS2_PLACEMENT_3D('',#7501,#5890,#5891);
#5233=AXIS2_PLACEMENT_3D('',#7503,#5892,#5893);
#5234=AXIS2_PLACEMENT_3D('',#7506,#5895,#5896);
#5235=AXIS2_PLACEMENT_3D('',#7507,#5897,#5898);
#5236=AXIS2_PLACEMENT_3D('',#7509,#5899,#5900);
#5237=AXIS2_PLACEMENT_3D('',#7512,#5902,#5903);
#5238=AXIS2_PLACEMENT_3D('',#7513,#5904,#5905);
#5239=AXIS2_PLACEMENT_3D('',#7522,#5910,#5911);
#5240=AXIS2_PLACEMENT_3D('',#7528,#5915,#5916);
#5241=AXIS2_PLACEMENT_3D('',#7534,#5920,#5921);
#5242=AXIS2_PLACEMENT_3D('',#7537,#5924,#5925);
#5243=AXIS2_PLACEMENT_3D('',#7538,#5926,#5927);
#5244=AXIS2_PLACEMENT_3D('',#7539,#5928,#5929);
#5245=AXIS2_PLACEMENT_3D('',#7540,#5930,#5931);
#5246=AXIS2_PLACEMENT_3D('',#7549,#5936,#5937);
#5247=AXIS2_PLACEMENT_3D('',#7555,#5941,#5942);
#5248=AXIS2_PLACEMENT_3D('',#7561,#5946,#5947);
#5249=AXIS2_PLACEMENT_3D('',#7564,#5950,#5951);
#5250=AXIS2_PLACEMENT_3D('',#7565,#5952,#5953);
#5251=AXIS2_PLACEMENT_3D('',#7566,#5954,#5955);
#5252=AXIS2_PLACEMENT_3D('',#7567,#5956,#5957);
#5253=AXIS2_PLACEMENT_3D('',#7576,#5962,#5963);
#5254=AXIS2_PLACEMENT_3D('',#7582,#5967,#5968);
#5255=AXIS2_PLACEMENT_3D('',#7588,#5972,#5973);
#5256=AXIS2_PLACEMENT_3D('',#7591,#5976,#5977);
#5257=AXIS2_PLACEMENT_3D('',#7592,#5978,#5979);
#5258=AXIS2_PLACEMENT_3D('',#7593,#5980,#5981);
#5259=AXIS2_PLACEMENT_3D('',#7594,#5982,#5983);
#5260=AXIS2_PLACEMENT_3D('',#7597,#5984,#5985);
#5261=AXIS2_PLACEMENT_3D('',#7598,#5986,#5987);
#5262=AXIS2_PLACEMENT_3D('',#7600,#5988,#5989);
#5263=AXIS2_PLACEMENT_3D('',#7601,#5990,#5991);
#5264=AXIS2_PLACEMENT_3D('',#7605,#5993,#5994);
#5265=AXIS2_PLACEMENT_3D('',#7607,#5996,#5997);
#5266=AXIS2_PLACEMENT_3D('',#7610,#5998,#5999);
#5267=AXIS2_PLACEMENT_3D('',#7611,#6000,#6001);
#5268=AXIS2_PLACEMENT_3D('',#7613,#6002,#6003);
#5269=AXIS2_PLACEMENT_3D('',#7614,#6004,#6005);
#5270=AXIS2_PLACEMENT_3D('',#7618,#6007,#6008);
#5271=AXIS2_PLACEMENT_3D('',#7620,#6010,#6011);
#5272=AXIS2_PLACEMENT_3D('',#7623,#6012,#6013);
#5273=AXIS2_PLACEMENT_3D('',#7624,#6014,#6015);
#5274=AXIS2_PLACEMENT_3D('',#7626,#6016,#6017);
#5275=AXIS2_PLACEMENT_3D('',#7627,#6018,#6019);
#5276=AXIS2_PLACEMENT_3D('',#7631,#6021,#6022);
#5277=AXIS2_PLACEMENT_3D('',#7633,#6024,#6025);
#5278=AXIS2_PLACEMENT_3D('',#7636,#6026,#6027);
#5279=AXIS2_PLACEMENT_3D('',#7637,#6028,#6029);
#5280=AXIS2_PLACEMENT_3D('',#7639,#6030,#6031);
#5281=AXIS2_PLACEMENT_3D('',#7640,#6032,#6033);
#5282=AXIS2_PLACEMENT_3D('',#7644,#6035,#6036);
#5283=AXIS2_PLACEMENT_3D('',#7646,#6038,#6039);
#5284=AXIS2_PLACEMENT_3D('',#7647,#6040,#6041);
#5285=AXIS2_PLACEMENT_3D('',#7648,#6042,#6043);
#5286=AXIS2_PLACEMENT_3D('',#7649,#6044,#6045);
#5287=AXIS2_PLACEMENT_3D('',#7651,#6046,#6047);
#5288=AXIS2_PLACEMENT_3D('',#7652,#6048,#6049);
#5289=AXIS2_PLACEMENT_3D('',#7654,#6050,#6051);
#5290=AXIS2_PLACEMENT_3D('',#7655,#6052,#6053);
#5291=AXIS2_PLACEMENT_3D('',#7658,#6055,#6056);
#5292=AXIS2_PLACEMENT_3D('',#7659,#6057,#6058);
#5293=AXIS2_PLACEMENT_3D('',#7661,#6059,#6060);
#5294=AXIS2_PLACEMENT_3D('',#7664,#6062,#6063);
#5295=AXIS2_PLACEMENT_3D('',#7665,#6064,#6065);
#5296=AXIS2_PLACEMENT_3D('',#7666,#6066,#6067);
#5297=AXIS2_PLACEMENT_3D('',#7679,#6074,#6075);
#5298=AXIS2_PLACEMENT_3D('',#7685,#6079,#6080);
#5299=AXIS2_PLACEMENT_3D('',#7691,#6084,#6085);
#5300=AXIS2_PLACEMENT_3D('',#7693,#6087,#6088);
#5301=AXIS2_PLACEMENT_3D('',#7699,#6092,#6093);
#5302=AXIS2_PLACEMENT_3D('',#7707,#6097,#6098);
#5303=AXIS2_PLACEMENT_3D('',#7709,#6100,#6101);
#5304=AXIS2_PLACEMENT_3D('',#7713,#6104,#6105);
#5305=AXIS2_PLACEMENT_3D('',#7719,#6109,#6110);
#5306=AXIS2_PLACEMENT_3D('',#7723,#6113,#6114);
#5307=AXIS2_PLACEMENT_3D('',#7725,#6116,#6117);
#5308=AXIS2_PLACEMENT_3D('',#7726,#6118,#6119);
#5309=AXIS2_PLACEMENT_3D('',#7727,#6120,#6121);
#5310=AXIS2_PLACEMENT_3D('',#7730,#6123,#6124);
#5311=AXIS2_PLACEMENT_3D('',#7735,#6126,#6127);
#5312=AXIS2_PLACEMENT_3D('',#7738,#6129,#6130);
#5313=AXIS2_PLACEMENT_3D('',#7743,#6132,#6133);
#5314=AXIS2_PLACEMENT_3D('',#7746,#6135,#6136);
#5315=AXIS2_PLACEMENT_3D('',#7747,#6137,#6138);
#5316=AXIS2_PLACEMENT_3D('',#7749,#6139,#6140);
#5317=AXIS2_PLACEMENT_3D('',#7752,#6142,#6143);
#5318=AXIS2_PLACEMENT_3D('',#7753,#6144,#6145);
#5319=AXIS2_PLACEMENT_3D('',#7762,#6150,#6151);
#5320=AXIS2_PLACEMENT_3D('',#7771,#6156,#6157);
#5321=AXIS2_PLACEMENT_3D('',#7777,#6161,#6162);
#5322=AXIS2_PLACEMENT_3D('',#7780,#6165,#6166);
#5323=AXIS2_PLACEMENT_3D('',#7784,#6169,#6170);
#5324=AXIS2_PLACEMENT_3D('',#7791,#6175,#6176);
#5325=AXIS2_PLACEMENT_3D('',#7797,#6180,#6181);
#5326=AXIS2_PLACEMENT_3D('',#7801,#6184,#6185);
#5327=AXIS2_PLACEMENT_3D('',#7804,#6188,#6189);
#5328=AXIS2_PLACEMENT_3D('',#7805,#6190,#6191);
#5329=AXIS2_PLACEMENT_3D('',#7806,#6192,#6193);
#5330=AXIS2_PLACEMENT_3D('',#7808,#6194,#6195);
#5331=AXIS2_PLACEMENT_3D('',#7811,#6197,#6198);
#5332=AXIS2_PLACEMENT_3D('',#7812,#6199,#6200);
#5333=AXIS2_PLACEMENT_3D('',#7825,#6207,#6208);
#5334=AXIS2_PLACEMENT_3D('',#7831,#6212,#6213);
#5335=AXIS2_PLACEMENT_3D('',#7837,#6217,#6218);
#5336=AXIS2_PLACEMENT_3D('',#7841,#6221,#6222);
#5337=AXIS2_PLACEMENT_3D('',#7843,#6224,#6225);
#5338=AXIS2_PLACEMENT_3D('',#7851,#6230,#6231);
#5339=AXIS2_PLACEMENT_3D('',#7856,#6235,#6236);
#5340=AXIS2_PLACEMENT_3D('',#7858,#6238,#6239);
#5341=AXIS2_PLACEMENT_3D('',#7862,#6242,#6243);
#5342=AXIS2_PLACEMENT_3D('',#7864,#6245,#6246);
#5343=AXIS2_PLACEMENT_3D('',#7865,#6247,#6248);
#5344=AXIS2_PLACEMENT_3D('',#7867,#6249,#6250);
#5345=AXIS2_PLACEMENT_3D('',#7869,#6252,#6253);
#5346=AXIS2_PLACEMENT_3D('',#7871,#6254,#6255);
#5347=AXIS2_PLACEMENT_3D('',#7873,#6257,#6258);
#5348=AXIS2_PLACEMENT_3D('',#7875,#6259,#6260);
#5349=AXIS2_PLACEMENT_3D('',#7877,#6262,#6263);
#5350=AXIS2_PLACEMENT_3D('',#7879,#6264,#6265);
#5351=AXIS2_PLACEMENT_3D('',#7881,#6267,#6268);
#5352=AXIS2_PLACEMENT_3D('',#7883,#6269,#6270);
#5353=AXIS2_PLACEMENT_3D('',#7885,#6271,#6272);
#5354=AXIS2_PLACEMENT_3D('',#7886,#6273,#6274);
#5355=AXIS2_PLACEMENT_3D('',#7888,#6275,#6276);
#5356=AXIS2_PLACEMENT_3D('',#7890,#6278,#6279);
#5357=AXIS2_PLACEMENT_3D('',#7891,#6280,#6281);
#5358=AXIS2_PLACEMENT_3D('',#7893,#6283,#6284);
#5359=AXIS2_PLACEMENT_3D('',#7894,#6285,#6286);
#5360=AXIS2_PLACEMENT_3D('',#7895,#6287,#6288);
#5361=AXIS2_PLACEMENT_3D('',#7904,#6293,#6294);
#5362=AXIS2_PLACEMENT_3D('',#7910,#6298,#6299);
#5363=AXIS2_PLACEMENT_3D('',#7916,#6303,#6304);
#5364=AXIS2_PLACEMENT_3D('',#7919,#6307,#6308);
#5365=AXIS2_PLACEMENT_3D('',#7920,#6309,#6310);
#5366=AXIS2_PLACEMENT_3D('',#7921,#6311,#6312);
#5367=AXIS2_PLACEMENT_3D('',#9143,#6313,#6314);
#5368=AXIS2_PLACEMENT_3D('',#9267,#6315,#6316);
#5369=AXIS2_PLACEMENT_3D('',#9268,#6317,#6318);
#5370=AXIS2_PLACEMENT_3D('',#9269,#6319,#6320);
#5371=AXIS2_PLACEMENT_3D('',#9270,#6321,#6322);
#5372=AXIS2_PLACEMENT_3D('',#9271,#6323,#6324);
#5373=AXIS2_PLACEMENT_3D('',#9280,#6329,#6330);
#5374=AXIS2_PLACEMENT_3D('',#9286,#6334,#6335);
#5375=AXIS2_PLACEMENT_3D('',#9292,#6339,#6340);
#5376=AXIS2_PLACEMENT_3D('',#9298,#6344,#6345);
#5377=AXIS2_PLACEMENT_3D('',#9304,#6349,#6350);
#5378=AXIS2_PLACEMENT_3D('',#9307,#6353,#6354);
#5379=AXIS2_PLACEMENT_3D('',#9308,#6355,#6356);
#5380=AXIS2_PLACEMENT_3D('',#9309,#6357,#6358);
#5381=AXIS2_PLACEMENT_3D('',#9311,#6359,#6360);
#5382=AXIS2_PLACEMENT_3D('',#9312,#6361,#6362);
#5383=AXIS2_PLACEMENT_3D('',#9314,#6363,#6364);
#5384=AXIS2_PLACEMENT_3D('',#9315,#6365,#6366);
#5385=AXIS2_PLACEMENT_3D('',#9317,#6367,#6368);
#5386=AXIS2_PLACEMENT_3D('',#9319,#6370,#6371);
#5387=AXIS2_PLACEMENT_3D('',#9321,#6372,#6373);
#5388=AXIS2_PLACEMENT_3D('',#9323,#6375,#6376);
#5389=AXIS2_PLACEMENT_3D('',#9325,#6377,#6378);
#5390=AXIS2_PLACEMENT_3D('',#9327,#6380,#6381);
#5391=AXIS2_PLACEMENT_3D('',#9329,#6382,#6383);
#5392=AXIS2_PLACEMENT_3D('',#9330,#6384,#6385);
#5393=AXIS2_PLACEMENT_3D('',#9332,#6386,#6387);
#5394=AXIS2_PLACEMENT_3D('',#9334,#6389,#6390);
#5395=AXIS2_PLACEMENT_3D('',#9336,#6392,#6393);
#5396=AXIS2_PLACEMENT_3D('',#9337,#6394,#6395);
#5397=AXIS2_PLACEMENT_3D('',#9338,#6396,#6397);
#5398=AXIS2_PLACEMENT_3D('',#9339,#6398,#6399);
#5399=AXIS2_PLACEMENT_3D('',#9340,#6400,#6401);
#5400=AXIS2_PLACEMENT_3D('',#9341,#6402,#6403);
#5401=AXIS2_PLACEMENT_3D('',#9342,#6404,#6405);
#5402=AXIS2_PLACEMENT_3D('',#9343,#6406,#6407);
#5403=AXIS2_PLACEMENT_3D('',#9344,#6408,#6409);
#5404=AXIS2_PLACEMENT_3D('',#9345,#6410,#6411);
#5405=AXIS2_PLACEMENT_3D('',#9346,#6412,#6413);
#5406=AXIS2_PLACEMENT_3D('',#9347,#6414,#6415);
#5407=AXIS2_PLACEMENT_3D('',#9348,#6416,#6417);
#5408=AXIS2_PLACEMENT_3D('',#9350,#6418,#6419);
#5409=AXIS2_PLACEMENT_3D('',#9353,#6421,#6422);
#5410=AXIS2_PLACEMENT_3D('',#9354,#6423,#6424);
#5411=AXIS2_PLACEMENT_3D('',#9355,#6425,#6426);
#5412=AXIS2_PLACEMENT_3D('',#9357,#6427,#6428);
#5413=AXIS2_PLACEMENT_3D('',#9360,#6430,#6431);
#5414=AXIS2_PLACEMENT_3D('',#9361,#6432,#6433);
#5415=AXIS2_PLACEMENT_3D('',#9362,#6434,#6435);
#5416=AXIS2_PLACEMENT_3D('',#9364,#6436,#6437);
#5417=AXIS2_PLACEMENT_3D('',#9367,#6439,#6440);
#5418=AXIS2_PLACEMENT_3D('',#9368,#6441,#6442);
#5419=AXIS2_PLACEMENT_3D('',#9369,#6443,#6444);
#5420=AXIS2_PLACEMENT_3D('',#9371,#6445,#6446);
#5421=AXIS2_PLACEMENT_3D('',#9374,#6448,#6449);
#5422=AXIS2_PLACEMENT_3D('',#9375,#6450,#6451);
#5423=AXIS2_PLACEMENT_3D('',#9376,#6452,#6453);
#5424=AXIS2_PLACEMENT_3D('',#9378,#6454,#6455);
#5425=AXIS2_PLACEMENT_3D('',#9381,#6457,#6458);
#5426=AXIS2_PLACEMENT_3D('',#9382,#6459,#6460);
#5427=AXIS2_PLACEMENT_3D('',#9383,#6461,#6462);
#5428=AXIS2_PLACEMENT_3D('',#9385,#6463,#6464);
#5429=AXIS2_PLACEMENT_3D('',#9388,#6466,#6467);
#5430=AXIS2_PLACEMENT_3D('',#9389,#6468,#6469);
#5431=AXIS2_PLACEMENT_3D('',#9390,#6470,#6471);
#5432=AXIS2_PLACEMENT_3D('',#9392,#6472,#6473);
#5433=AXIS2_PLACEMENT_3D('',#9395,#6475,#6476);
#5434=AXIS2_PLACEMENT_3D('',#9396,#6477,#6478);
#5435=AXIS2_PLACEMENT_3D('',#9397,#6479,#6480);
#5436=AXIS2_PLACEMENT_3D('',#9399,#6481,#6482);
#5437=AXIS2_PLACEMENT_3D('',#9402,#6484,#6485);
#5438=AXIS2_PLACEMENT_3D('',#9403,#6486,#6487);
#5439=AXIS2_PLACEMENT_3D('',#9404,#6488,#6489);
#5440=AXIS2_PLACEMENT_3D('',#9406,#6490,#6491);
#5441=AXIS2_PLACEMENT_3D('',#9409,#6493,#6494);
#5442=AXIS2_PLACEMENT_3D('',#9410,#6495,#6496);
#5443=AXIS2_PLACEMENT_3D('',#9411,#6497,#6498);
#5444=AXIS2_PLACEMENT_3D('',#9416,#6500,#6501);
#5445=AXIS2_PLACEMENT_3D('',#9419,#6503,#6504);
#5446=AXIS2_PLACEMENT_3D('',#9420,#6505,#6506);
#5447=AXIS2_PLACEMENT_3D('',#9424,#6508,#6509);
#5448=AXIS2_PLACEMENT_3D('',#9426,#6511,#6512);
#5449=AXIS2_PLACEMENT_3D('',#9430,#6515,#6516);
#5450=AXIS2_PLACEMENT_3D('',#9434,#6519,#6520);
#5451=AXIS2_PLACEMENT_3D('',#9435,#6521,#6522);
#5452=AXIS2_PLACEMENT_3D('',#9436,#6523,#6524);
#5453=AXIS2_PLACEMENT_3D('',#9438,#6525,#6526);
#5454=AXIS2_PLACEMENT_3D('',#9441,#6528,#6529);
#5455=AXIS2_PLACEMENT_3D('',#9442,#6530,#6531);
#5456=AXIS2_PLACEMENT_3D('',#9444,#6532,#6533);
#5457=AXIS2_PLACEMENT_3D('',#9447,#6535,#6536);
#5458=AXIS2_PLACEMENT_3D('',#9448,#6537,#6538);
#5459=AXIS2_PLACEMENT_3D('',#9449,#6539,#6540);
#5460=AXIS2_PLACEMENT_3D('',#9450,#6541,#6542);
#5461=AXIS2_PLACEMENT_3D('',#9451,#6543,#6544);
#5462=AXIS2_PLACEMENT_3D('',#9453,#6545,#6546);
#5463=AXIS2_PLACEMENT_3D('',#9456,#6548,#6549);
#5464=AXIS2_PLACEMENT_3D('',#9457,#6550,#6551);
#5465=AXIS2_PLACEMENT_3D('',#9459,#6552,#6553);
#5466=AXIS2_PLACEMENT_3D('',#9462,#6555,#6556);
#5467=AXIS2_PLACEMENT_3D('',#9463,#6557,#6558);
#5468=AXIS2_PLACEMENT_3D('',#9464,#6559,#6560);
#5469=AXIS2_PLACEMENT_3D('',#9465,#6561,#6562);
#5470=AXIS2_PLACEMENT_3D('',#9466,#6563,#6564);
#5471=AXIS2_PLACEMENT_3D('',#9468,#6565,#6566);
#5472=AXIS2_PLACEMENT_3D('',#9471,#6568,#6569);
#5473=AXIS2_PLACEMENT_3D('',#9472,#6570,#6571);
#5474=AXIS2_PLACEMENT_3D('',#9474,#6572,#6573);
#5475=AXIS2_PLACEMENT_3D('',#9477,#6575,#6576);
#5476=AXIS2_PLACEMENT_3D('',#9478,#6577,#6578);
#5477=AXIS2_PLACEMENT_3D('',#9479,#6579,#6580);
#5478=AXIS2_PLACEMENT_3D('',#9480,#6581,#6582);
#5479=AXIS2_PLACEMENT_3D('',#9481,#6583,#6584);
#5480=AXIS2_PLACEMENT_3D('',#9483,#6585,#6586);
#5481=AXIS2_PLACEMENT_3D('',#9486,#6588,#6589);
#5482=AXIS2_PLACEMENT_3D('',#9487,#6590,#6591);
#5483=AXIS2_PLACEMENT_3D('',#9489,#6592,#6593);
#5484=AXIS2_PLACEMENT_3D('',#9490,#6594,#6595);
#5485=AXIS2_PLACEMENT_3D('',#9492,#6596,#6597);
#5486=AXIS2_PLACEMENT_3D('',#9495,#6599,#6600);
#5487=AXIS2_PLACEMENT_3D('',#9496,#6601,#6602);
#5488=AXIS2_PLACEMENT_3D('',#9498,#6603,#6604);
#5489=AXIS2_PLACEMENT_3D('',#9499,#6605,#6606);
#5490=AXIS2_PLACEMENT_3D('',#9501,#6607,#6608);
#5491=AXIS2_PLACEMENT_3D('',#9504,#6610,#6611);
#5492=AXIS2_PLACEMENT_3D('',#9505,#6612,#6613);
#5493=AXIS2_PLACEMENT_3D('',#9507,#6614,#6615);
#5494=AXIS2_PLACEMENT_3D('',#9508,#6616,#6617);
#5495=AXIS2_PLACEMENT_3D('',#9510,#6618,#6619);
#5496=AXIS2_PLACEMENT_3D('',#9513,#6621,#6622);
#5497=AXIS2_PLACEMENT_3D('',#9514,#6623,#6624);
#5498=AXIS2_PLACEMENT_3D('',#9516,#6625,#6626);
#5499=AXIS2_PLACEMENT_3D('',#9517,#6627,#6628);
#5500=AXIS2_PLACEMENT_3D('',#9520,#6630,#6631);
#5501=AXIS2_PLACEMENT_3D('',#9521,#6632,#6633);
#5502=AXIS2_PLACEMENT_3D('',#9524,#6635,#6636);
#5503=AXIS2_PLACEMENT_3D('',#9525,#6637,#6638);
#5504=AXIS2_PLACEMENT_3D('',#9528,#6640,#6641);
#5505=AXIS2_PLACEMENT_3D('',#9529,#6642,#6643);
#5506=AXIS2_PLACEMENT_3D('',#9532,#6645,#6646);
#5507=AXIS2_PLACEMENT_3D('',#9533,#6647,#6648);
#5508=AXIS2_PLACEMENT_3D('',#9535,#6649,#6650);
#5509=AXIS2_PLACEMENT_3D('',#9538,#6652,#6653);
#5510=AXIS2_PLACEMENT_3D('',#9539,#6654,#6655);
#5511=AXIS2_PLACEMENT_3D('',#9541,#6656,#6657);
#5512=AXIS2_PLACEMENT_3D('',#9542,#6658,#6659);
#5513=AXIS2_PLACEMENT_3D('',#9545,#6661,#6662);
#5514=AXIS2_PLACEMENT_3D('',#9546,#6663,#6664);
#5515=AXIS2_PLACEMENT_3D('',#9548,#6665,#6666);
#5516=AXIS2_PLACEMENT_3D('',#9551,#6668,#6669);
#5517=AXIS2_PLACEMENT_3D('',#9552,#6670,#6671);
#5518=AXIS2_PLACEMENT_3D('',#9553,#6672,#6673);
#5519=AXIS2_PLACEMENT_3D('',#9554,#6674,#6675);
#5520=AXIS2_PLACEMENT_3D('',#9555,#6676,#6677);
#5521=AXIS2_PLACEMENT_3D('',#9557,#6678,#6679);
#5522=AXIS2_PLACEMENT_3D('',#9560,#6681,#6682);
#5523=AXIS2_PLACEMENT_3D('',#9561,#6683,#6684);
#5524=AXIS2_PLACEMENT_3D('',#9563,#6685,#6686);
#5525=AXIS2_PLACEMENT_3D('',#9564,#6687,#6688);
#5526=AXIS2_PLACEMENT_3D('',#9566,#6689,#6690);
#5527=AXIS2_PLACEMENT_3D('',#9569,#6692,#6693);
#5528=AXIS2_PLACEMENT_3D('',#9570,#6694,#6695);
#5529=AXIS2_PLACEMENT_3D('',#9572,#6696,#6697);
#5530=AXIS2_PLACEMENT_3D('',#9573,#6698,#6699);
#5531=AXIS2_PLACEMENT_3D('',#9575,#6700,#6701);
#5532=AXIS2_PLACEMENT_3D('',#9578,#6703,#6704);
#5533=AXIS2_PLACEMENT_3D('',#9579,#6705,#6706);
#5534=AXIS2_PLACEMENT_3D('',#9581,#6707,#6708);
#5535=AXIS2_PLACEMENT_3D('',#9582,#6709,#6710);
#5536=AXIS2_PLACEMENT_3D('',#9584,#6711,#6712);
#5537=AXIS2_PLACEMENT_3D('',#9587,#6714,#6715);
#5538=AXIS2_PLACEMENT_3D('',#9588,#6716,#6717);
#5539=AXIS2_PLACEMENT_3D('',#9590,#6718,#6719);
#5540=AXIS2_PLACEMENT_3D('',#9591,#6720,#6721);
#5541=AXIS2_PLACEMENT_3D('',#9593,#6722,#6723);
#5542=AXIS2_PLACEMENT_3D('',#9595,#6725,#6726);
#5543=AXIS2_PLACEMENT_3D('',#9597,#6727,#6728);
#5544=AXIS2_PLACEMENT_3D('',#9599,#6730,#6731);
#5545=AXIS2_PLACEMENT_3D('',#9601,#6732,#6733);
#5546=AXIS2_PLACEMENT_3D('',#9603,#6735,#6736);
#5547=AXIS2_PLACEMENT_3D('',#9605,#6737,#6738);
#5548=AXIS2_PLACEMENT_3D('',#9607,#6740,#6741);
#5549=AXIS2_PLACEMENT_3D('',#9616,#6746,#6747);
#5550=AXIS2_PLACEMENT_3D('',#9625,#6752,#6753);
#5551=AXIS2_PLACEMENT_3D('',#9628,#6756,#6757);
#5552=AXIS2_PLACEMENT_3D('',#9630,#6758,#6759);
#5553=AXIS2_PLACEMENT_3D('',#9633,#6761,#6762);
#5554=AXIS2_PLACEMENT_3D('',#9634,#6763,#6764);
#5555=AXIS2_PLACEMENT_3D('',#9636,#6765,#6766);
#5556=AXIS2_PLACEMENT_3D('',#9637,#6767,#6768);
#5557=AXIS2_PLACEMENT_3D('',#9639,#6769,#6770);
#5558=AXIS2_PLACEMENT_3D('',#9641,#6772,#6773);
#5559=AXIS2_PLACEMENT_3D('',#9642,#6774,#6775);
#5560=AXIS2_PLACEMENT_3D('',#9643,#6776,#6777);
#5561=AXIS2_PLACEMENT_3D('',#9644,#6778,#6779);
#5562=AXIS2_PLACEMENT_3D('',#9645,#6780,#6781);
#5563=AXIS2_PLACEMENT_3D('',#9646,#6782,#6783);
#5564=AXIS2_PLACEMENT_3D('',#9647,#6784,#6785);
#5565=AXIS2_PLACEMENT_3D('',#9649,#6786,#6787);
#5566=AXIS2_PLACEMENT_3D('',#9652,#6789,#6790);
#5567=AXIS2_PLACEMENT_3D('',#9653,#6791,#6792);
#5568=AXIS2_PLACEMENT_3D('',#9654,#6793,#6794);
#5569=AXIS2_PLACEMENT_3D('',#9656,#6795,#6796);
#5570=AXIS2_PLACEMENT_3D('',#9659,#6798,#6799);
#5571=AXIS2_PLACEMENT_3D('',#9660,#6800,#6801);
#5572=AXIS2_PLACEMENT_3D('',#9661,#6802,#6803);
#5573=AXIS2_PLACEMENT_3D('',#9662,#6804,#6805);
#5574=AXIS2_PLACEMENT_3D('',#9663,#6806,#6807);
#5575=AXIS2_PLACEMENT_3D('',#9665,#6808,#6809);
#5576=AXIS2_PLACEMENT_3D('',#9668,#6811,#6812);
#5577=AXIS2_PLACEMENT_3D('',#9669,#6813,#6814);
#5578=AXIS2_PLACEMENT_3D('',#9670,#6815,#6816);
#5579=AXIS2_PLACEMENT_3D('',#9671,#6817,#6818);
#5580=AXIS2_PLACEMENT_3D('',#9672,#6819,#6820);
#5581=AXIS2_PLACEMENT_3D('',#9673,#6821,#6822);
#5582=AXIS2_PLACEMENT_3D('',#9676,#6823,#6824);
#5583=AXIS2_PLACEMENT_3D('',#9677,#6825,#6826);
#5584=AXIS2_PLACEMENT_3D('',#9679,#6827,#6828);
#5585=AXIS2_PLACEMENT_3D('',#9681,#6829,#6830);
#5586=AXIS2_PLACEMENT_3D('',#9682,#6831,#6832);
#5587=AXIS2_PLACEMENT_3D('',#9683,#6833,#6834);
#5588=AXIS2_PLACEMENT_3D('',#9686,#6836,#6837);
#5589=AXIS2_PLACEMENT_3D('',#9687,#6838,#6839);
#5590=AXIS2_PLACEMENT_3D('',#9689,#6840,#6841);
#5591=AXIS2_PLACEMENT_3D('',#9692,#6843,#6844);
#5592=AXIS2_PLACEMENT_3D('',#9693,#6845,#6846);
#5593=AXIS2_PLACEMENT_3D('',#9696,#6848,#6849);
#5594=AXIS2_PLACEMENT_3D('',#9697,#6850,#6851);
#5595=AXIS2_PLACEMENT_3D('',#9698,#6852,#6853);
#5596=AXIS2_PLACEMENT_3D('',#9700,#6854,#6855);
#5597=AXIS2_PLACEMENT_3D('',#9702,#6857,#6858);
#5598=AXIS2_PLACEMENT_3D('',#9704,#6859,#6860);
#5599=AXIS2_PLACEMENT_3D('',#9705,#6861,#6862);
#5600=AXIS2_PLACEMENT_3D('',#9707,#6864,#6865);
#5601=AXIS2_PLACEMENT_3D('',#9708,#6866,#6867);
#5602=AXIS2_PLACEMENT_3D('',#9711,#6868,#6869);
#5603=AXIS2_PLACEMENT_3D('',#9712,#6870,#6871);
#5604=AXIS2_PLACEMENT_3D('',#9714,#6872,#6873);
#5605=AXIS2_PLACEMENT_3D('',#9716,#6874,#6875);
#5606=AXIS2_PLACEMENT_3D('',#9717,#6876,#6877);
#5607=AXIS2_PLACEMENT_3D('',#9718,#6878,#6879);
#5608=AXIS2_PLACEMENT_3D('',#9720,#6880,#6881);
#5609=AXIS2_PLACEMENT_3D('',#9722,#6883,#6884);
#5610=AXIS2_PLACEMENT_3D('',#9724,#6885,#6886);
#5611=AXIS2_PLACEMENT_3D('',#9726,#6887,#6888);
#5612=AXIS2_PLACEMENT_3D('',#9727,#6889,#6890);
#5613=AXIS2_PLACEMENT_3D('',#9729,#6891,#6892);
#5614=AXIS2_PLACEMENT_3D('',#9731,#6894,#6895);
#5615=AXIS2_PLACEMENT_3D('',#9733,#6896,#6897);
#5616=AXIS2_PLACEMENT_3D('',#9735,#6899,#6900);
#5617=AXIS2_PLACEMENT_3D('',#9737,#6901,#6902);
#5618=AXIS2_PLACEMENT_3D('',#9739,#6904,#6905);
#5619=AXIS2_PLACEMENT_3D('',#9740,#6906,#6907);
#5620=AXIS2_PLACEMENT_3D('',#9742,#6909,#6910);
#5621=AXIS2_PLACEMENT_3D('',#9743,#6911,#6912);
#5622=AXIS2_PLACEMENT_3D('',#9746,#6913,#6914);
#5623=AXIS2_PLACEMENT_3D('',#9747,#6915,#6916);
#5624=AXIS2_PLACEMENT_3D('',#9750,#6917,#6918);
#5625=AXIS2_PLACEMENT_3D('',#9751,#6919,#6920);
#5626=AXIS2_PLACEMENT_3D('',#9754,#6921,#6922);
#5627=AXIS2_PLACEMENT_3D('',#9755,#6923,#6924);
#5628=AXIS2_PLACEMENT_3D('',#9758,#6925,#6926);
#5629=AXIS2_PLACEMENT_3D('',#9759,#6927,#6928);
#5630=AXIS2_PLACEMENT_3D('',#9762,#6929,#6930);
#5631=AXIS2_PLACEMENT_3D('',#9763,#6931,#6932);
#5632=AXIS2_PLACEMENT_3D('',#9766,#6933,#6934);
#5633=AXIS2_PLACEMENT_3D('',#9767,#6935,#6936);
#5634=AXIS2_PLACEMENT_3D('',#9770,#6937,#6938);
#5635=AXIS2_PLACEMENT_3D('',#9771,#6939,#6940);
#5636=AXIS2_PLACEMENT_3D('',#9774,#6941,#6942);
#5637=AXIS2_PLACEMENT_3D('',#9775,#6943,#6944);
#5638=AXIS2_PLACEMENT_3D('',#9776,#6945,#6946);
#5639=AXIS2_PLACEMENT_3D('',#9802,#6947,#6948);
#5640=AXIS2_PLACEMENT_3D('',#9826,#6949,#6950);
#5641=AXIS2_PLACEMENT_3D('',#9827,#6951,#6952);
#5642=AXIS2_PLACEMENT_3D('',#9829,#6953,#6954);
#5643=AXIS2_PLACEMENT_3D('',#9854,#6955,#6956);
#5644=AXIS2_PLACEMENT_3D('',#9879,#6957,#6958);
#5645=AXIS2_PLACEMENT_3D('',#9895,#6960,#6961);
#5646=AXIS2_PLACEMENT_3D('',#9910,#6962,#6963);
#5647=AXIS2_PLACEMENT_3D('',#9935,#6964,#6965);
#5648=AXIS2_PLACEMENT_3D('',#9960,#6966,#6967);
#5649=AXIS2_PLACEMENT_3D('',#9985,#6968,#6969);
#5650=AXIS2_PLACEMENT_3D('',#10009,#6970,#6971);
#5651=AXIS2_PLACEMENT_3D('',#10010,#6972,#6973);
#5652=AXIS2_PLACEMENT_3D('',#10012,#6974,#6975);
#5653=AXIS2_PLACEMENT_3D('',#10013,#6976,#6977);
#5654=AXIS2_PLACEMENT_3D('',#10014,#6978,#6979);
#5655=AXIS2_PLACEMENT_3D('',#10038,#6980,#6981);
#5656=AXIS2_PLACEMENT_3D('',#10039,#6982,#6983);
#5657=AXIS2_PLACEMENT_3D('',#10041,#6984,#6985);
#5658=AXIS2_PLACEMENT_3D('',#10042,#6986,#6987);
#5659=AXIS2_PLACEMENT_3D('',#10043,#6988,#6989);
#5660=AXIS2_PLACEMENT_3D('',#10067,#6990,#6991);
#5661=AXIS2_PLACEMENT_3D('',#10068,#6992,#6993);
#5662=AXIS2_PLACEMENT_3D('',#10070,#6994,#6995);
#5663=AXIS2_PLACEMENT_3D('',#10071,#6996,#6997);
#5664=AXIS2_PLACEMENT_3D('',#10072,#6998,#6999);
#5665=AXIS2_PLACEMENT_3D('',#10087,#7000,#7001);
#5666=AXIS2_PLACEMENT_3D('',#10100,#7002,#7003);
#5667=AXIS2_PLACEMENT_3D('',#10102,#7004,#7005);
#5668=AXIS2_PLACEMENT_3D('',#10103,#7006,#7007);
#5669=AXIS2_PLACEMENT_3D('',#10104,#7008,#7009);
#5670=AXIS2_PLACEMENT_3D('',#10128,#7010,#7011);
#5671=AXIS2_PLACEMENT_3D('',#10129,#7012,#7013);
#5672=AXIS2_PLACEMENT_3D('',#10131,#7014,#7015);
#5673=AXIS2_PLACEMENT_3D('',#10132,#7016,#7017);
#5674=AXIS2_PLACEMENT_3D('',#10133,#7018,#7019);
#5675=AXIS2_PLACEMENT_3D('',#10157,#7020,#7021);
#5676=AXIS2_PLACEMENT_3D('',#10158,#7022,#7023);
#5677=AXIS2_PLACEMENT_3D('',#10160,#7024,#7025);
#5678=AXIS2_PLACEMENT_3D('',#10161,#7026,#7027);
#5679=AXIS2_PLACEMENT_3D('',#10162,#7028,#7029);
#5680=AXIS2_PLACEMENT_3D('',#10186,#7030,#7031);
#5681=AXIS2_PLACEMENT_3D('',#10187,#7032,#7033);
#5682=AXIS2_PLACEMENT_3D('',#10189,#7034,#7035);
#5683=AXIS2_PLACEMENT_3D('',#10192,#7037,#7038);
#5684=AXIS2_PLACEMENT_3D('',#10216,#7039,#7040);
#5685=AXIS2_PLACEMENT_3D('',#10217,#7041,#7042);
#5686=AXIS2_PLACEMENT_3D('',#10218,#7043,#7044);
#5687=AXIS2_PLACEMENT_3D('',#10219,#7045,#7046);
#5688=AXIS2_PLACEMENT_3D('',#10220,#7047,#7048);
#5689=AXIS2_PLACEMENT_3D('',#10221,#7049,#7050);
#5690=AXIS2_PLACEMENT_3D('',#10222,#7051,#7052);
#5691=AXIS2_PLACEMENT_3D('',#10223,#7053,#7054);
#5692=AXIS2_PLACEMENT_3D('',#10224,#7055,#7056);
#5693=AXIS2_PLACEMENT_3D('',#10226,#7057,#7058);
#5694=AXIS2_PLACEMENT_3D('',#10228,#7059,#7060);
#5695=AXIS2_PLACEMENT_3D('',#10229,#7061,#7062);
#5696=AXIS2_PLACEMENT_3D('',#10231,#7063,#7064);
#5697=AXIS2_PLACEMENT_3D('',#10233,#7066,#7067);
#5698=AXIS2_PLACEMENT_3D('',#10235,#7068,#7069);
#5699=AXIS2_PLACEMENT_3D('',#10236,#7070,#7071);
#5700=AXIS2_PLACEMENT_3D('',#10238,#7073,#7074);
#5701=AXIS2_PLACEMENT_3D('',#10240,#7075,#7076);
#5702=AXIS2_PLACEMENT_3D('',#10242,#7077,#7078);
#5703=AXIS2_PLACEMENT_3D('',#10243,#7079,#7080);
#5704=AXIS2_PLACEMENT_3D('',#10245,#7081,#7082);
#5705=AXIS2_PLACEMENT_3D('',#10247,#7084,#7085);
#5706=AXIS2_PLACEMENT_3D('',#10249,#7086,#7087);
#5707=AXIS2_PLACEMENT_3D('',#10250,#7088,#7089);
#5708=AXIS2_PLACEMENT_3D('',#10252,#7091,#7092);
#5709=AXIS2_PLACEMENT_3D('',#10253,#7093,#7094);
#5710=AXIS2_PLACEMENT_3D('',#10254,#7095,#7096);
#5711=AXIS2_PLACEMENT_3D('',#10255,#7097,#7098);
#5712=AXIS2_PLACEMENT_3D('',#10256,#7099,#7100);
#5713=AXIS2_PLACEMENT_3D('',#10257,#7101,#7102);
#5714=AXIS2_PLACEMENT_3D('',#10258,#7103,#7104);
#5715=AXIS2_PLACEMENT_3D('',#10259,#7105,#7106);
#5716=AXIS2_PLACEMENT_3D('',#10261,#7107,#7108);
#5717=AXIS2_PLACEMENT_3D('',#10264,#7110,#7111);
#5718=AXIS2_PLACEMENT_3D('',#10265,#7112,#7113);
#5719=AXIS2_PLACEMENT_3D('',#10266,#7114,#7115);
#5720=AXIS2_PLACEMENT_3D('',#10268,#7116,#7117);
#5721=AXIS2_PLACEMENT_3D('',#10271,#7119,#7120);
#5722=AXIS2_PLACEMENT_3D('',#10272,#7121,#7122);
#5723=AXIS2_PLACEMENT_3D('',#10273,#7123,#7124);
#5724=AXIS2_PLACEMENT_3D('',#10275,#7125,#7126);
#5725=AXIS2_PLACEMENT_3D('',#10277,#7127,#7128);
#5726=AXIS2_PLACEMENT_3D('',#10278,#7129,#7130);
#5727=AXIS2_PLACEMENT_3D('',#10281,#7132,#7133);
#5728=AXIS2_PLACEMENT_3D('',#10282,#7134,#7135);
#5729=AXIS2_PLACEMENT_3D('',#10284,#7136,#7137);
#5730=AXIS2_PLACEMENT_3D('',#10286,#7138,#7139);
#5731=AXIS2_PLACEMENT_3D('',#10287,#7140,#7141);
#5732=AXIS2_PLACEMENT_3D('',#10289,#7142,#7143);
#5733=AXIS2_PLACEMENT_3D('',#10291,#7145,#7146);
#5734=AXIS2_PLACEMENT_3D('',#10294,#7148,#7149);
#5735=AXIS2_PLACEMENT_3D('',#10295,#7150,#7151);
#5736=AXIS2_PLACEMENT_3D('',#10297,#7152,#7153);
#5737=AXIS2_PLACEMENT_3D('',#10299,#7155,#7156);
#5738=AXIS2_PLACEMENT_3D('',#10300,#7157,#7158);
#5739=AXIS2_PLACEMENT_3D('',#10301,#7159,#7160);
#5740=AXIS2_PLACEMENT_3D('',#10303,#7161,#7162);
#5741=AXIS2_PLACEMENT_3D('',#10306,#7164,#7165);
#5742=AXIS2_PLACEMENT_3D('',#10307,#7166,#7167);
#5743=AXIS2_PLACEMENT_3D('',#10308,#7168,#7169);
#5744=AXIS2_PLACEMENT_3D('',#10309,#7170,#7171);
#5745=AXIS2_PLACEMENT_3D('',#10310,#7172,#7173);
#5746=AXIS2_PLACEMENT_3D('',#10312,#7174,#7175);
#5747=AXIS2_PLACEMENT_3D('',#10315,#7177,#7178);
#5748=AXIS2_PLACEMENT_3D('',#10316,#7179,#7180);
#5749=AXIS2_PLACEMENT_3D('',#10321,#7182,#7183);
#5750=AXIS2_PLACEMENT_3D('',#10324,#7185,#7186);
#5751=AXIS2_PLACEMENT_3D('',#10325,#7187,#7188);
#5752=AXIS2_PLACEMENT_3D('',#10329,#7190,#7191);
#5753=AXIS2_PLACEMENT_3D('',#10331,#7192,#7193);
#5754=AXIS2_PLACEMENT_3D('',#10334,#7195,#7196);
#5755=AXIS2_PLACEMENT_3D('',#10335,#7197,#7198);
#5756=AXIS2_PLACEMENT_3D('',#10339,#7201,#7202);
#5757=AXIS2_PLACEMENT_3D('',#10343,#7205,#7206);
#5758=AXIS2_PLACEMENT_3D('',#10344,#7207,#7208);
#5759=AXIS2_PLACEMENT_3D('',#10345,#7209,#7210);
#5760=AXIS2_PLACEMENT_3D('',#10347,#7211,#7212);
#5761=AXIS2_PLACEMENT_3D('',#10349,#7214,#7215);
#5762=AXIS2_PLACEMENT_3D('',#10351,#7216,#7217);
#5763=AXIS2_PLACEMENT_3D('',#10353,#7219,#7220);
#5764=AXIS2_PLACEMENT_3D('',#10354,#7221,#7222);
#5765=AXIS2_PLACEMENT_3D('',#10355,#7223,#7224);
#5766=AXIS2_PLACEMENT_3D('',#10357,#7225,#7226);
#5767=AXIS2_PLACEMENT_3D('',#10360,#7228,#7229);
#5768=AXIS2_PLACEMENT_3D('',#10361,#7230,#7231);
#5769=AXIS2_PLACEMENT_3D('',#10362,#7232,#7233);
#5770=AXIS2_PLACEMENT_3D('',#10364,#7234,#7235);
#5771=AXIS2_PLACEMENT_3D('',#10367,#7237,#7238);
#5772=AXIS2_PLACEMENT_3D('',#10368,#7239,#7240);
#5773=AXIS2_PLACEMENT_3D('',#10369,#7241,#7242);
#5774=AXIS2_PLACEMENT_3D('',#10370,#7243,#7244);
#5775=AXIS2_PLACEMENT_3D('',#10371,#7245,#7246);
#5776=AXIS2_PLACEMENT_3D('',#10373,#7247,#7248);
#5777=AXIS2_PLACEMENT_3D('',#10376,#7250,#7251);
#5778=AXIS2_PLACEMENT_3D('',#10377,#7252,#7253);
#5779=AXIS2_PLACEMENT_3D('',#10379,#7254,#7255);
#5780=AXIS2_PLACEMENT_3D('',#10382,#7257,#7258);
#5781=AXIS2_PLACEMENT_3D('',#10383,#7259,#7260);
#5782=AXIS2_PLACEMENT_3D('',#10384,#7261,#7262);
#5783=AXIS2_PLACEMENT_3D('',#10385,#7263,#7264);
#5784=AXIS2_PLACEMENT_3D('',#10386,#7265,#7266);
#5785=AXIS2_PLACEMENT_3D('',#10388,#7267,#7268);
#5786=AXIS2_PLACEMENT_3D('',#10391,#7270,#7271);
#5787=AXIS2_PLACEMENT_3D('',#10392,#7272,#7273);
#5788=AXIS2_PLACEMENT_3D('',#10394,#7274,#7275);
#5789=AXIS2_PLACEMENT_3D('',#10397,#7277,#7278);
#5790=AXIS2_PLACEMENT_3D('',#10398,#7279,#7280);
#5791=AXIS2_PLACEMENT_3D('',#10399,#7281,#7282);
#5792=AXIS2_PLACEMENT_3D('',#10400,#7283,#7284);
#5793=AXIS2_PLACEMENT_3D('',#10401,#7285,#7286);
#5794=AXIS2_PLACEMENT_3D('',#10403,#7287,#7288);
#5795=AXIS2_PLACEMENT_3D('',#10404,#7289,#7290);
#5796=AXIS2_PLACEMENT_3D('',#10406,#7291,#7292);
#5797=AXIS2_PLACEMENT_3D('',#10408,#7294,#7295);
#5798=AXIS2_PLACEMENT_3D('',#10410,#7296,#7297);
#5799=AXIS2_PLACEMENT_3D('',#10412,#7299,#7300);
#5800=AXIS2_PLACEMENT_3D('',#10414,#7301,#7302);
#5801=AXIS2_PLACEMENT_3D('',#10416,#7304,#7305);
#5802=AXIS2_PLACEMENT_3D('',#10418,#7306,#7307);
#5803=AXIS2_PLACEMENT_3D('',#10419,#7308,#7309);
#5804=AXIS2_PLACEMENT_3D('',#10421,#7310,#7311);
#5805=AXIS2_PLACEMENT_3D('',#10423,#7313,#7314);
#5806=AXIS2_PLACEMENT_3D('',#10425,#7315,#7316);
#5807=AXIS2_PLACEMENT_3D('',#10427,#7318,#7319);
#5808=AXIS2_PLACEMENT_3D('',#10429,#7320,#7321);
#5809=AXIS2_PLACEMENT_3D('',#10431,#7323,#7324);
#5810=AXIS2_PLACEMENT_3D('',#10432,#7325,#7326);
#5811=AXIS2_PLACEMENT_3D('',#10441,#7331,#7332);
#5812=AXIS2_PLACEMENT_3D('',#10447,#7336,#7337);
#5813=AXIS2_PLACEMENT_3D('',#10453,#7341,#7342);
#5814=AXIS2_PLACEMENT_3D('',#10459,#7346,#7347);
#5815=AXIS2_PLACEMENT_3D('',#10465,#7351,#7352);
#5816=AXIS2_PLACEMENT_3D('',#10468,#7355,#7356);
#5817=AXIS2_PLACEMENT_3D('',#10469,#7357,#7358);
#5818=AXIS2_PLACEMENT_3D('',#10470,#7359,#7360);
#5819=AXIS2_PLACEMENT_3D('',#10471,#7361,#7362);
#5820=AXIS2_PLACEMENT_3D('',#10480,#7367,#7368);
#5821=AXIS2_PLACEMENT_3D('',#10486,#7372,#7373);
#5822=AXIS2_PLACEMENT_3D('',#10492,#7377,#7378);
#5823=AXIS2_PLACEMENT_3D('',#10498,#7382,#7383);
#5824=AXIS2_PLACEMENT_3D('',#10504,#7387,#7388);
#5825=AXIS2_PLACEMENT_3D('',#10507,#7391,#7392);
#5826=AXIS2_PLACEMENT_3D('',#10508,#7393,#7394);
#5827=AXIS2_PLACEMENT_3D('',#10509,#7395,#7396);
#5828=AXIS2_PLACEMENT_3D('',#10511,#7397,#7398);
#5829=AXIS2_PLACEMENT_3D('',#10512,#7399,#7400);
#5830=AXIS2_PLACEMENT_3D('',#10514,#7401,#7402);
#5831=AXIS2_PLACEMENT_3D('',#10515,#7403,#7404);
#5832=AXIS2_PLACEMENT_3D('',#10517,#7405,#7406);
#5833=AXIS2_PLACEMENT_3D('',#10519,#7408,#7409);
#5834=AXIS2_PLACEMENT_3D('',#10521,#7410,#7411);
#5835=AXIS2_PLACEMENT_3D('',#10523,#7413,#7414);
#5836=AXIS2_PLACEMENT_3D('',#10525,#7415,#7416);
#5837=AXIS2_PLACEMENT_3D('',#10527,#7418,#7419);
#5838=AXIS2_PLACEMENT_3D('',#10529,#7420,#7421);
#5839=AXIS2_PLACEMENT_3D('',#10530,#7422,#7423);
#5840=AXIS2_PLACEMENT_3D('',#10532,#7424,#7425);
#5841=AXIS2_PLACEMENT_3D('',#10534,#7427,#7428);
#5842=AXIS2_PLACEMENT_3D('',#10536,#7430,#7431);
#5843=AXIS2_PLACEMENT_3D('',#10537,#7432,#7433);
#5844=AXIS2_PLACEMENT_3D('',#10538,#7434,#7435);
#5845=AXIS2_PLACEMENT_3D('',#10539,#7436,#7437);
#5846=AXIS2_PLACEMENT_3D('',#10540,#7438,#7439);
#5847=AXIS2_PLACEMENT_3D('',#10541,#7440,#7441);
#5848=AXIS2_PLACEMENT_3D('',#10542,#7442,#7443);
#5849=AXIS2_PLACEMENT_3D('',#10543,#7444,#7445);
#5850=AXIS2_PLACEMENT_3D('',#10544,#7446,#7447);
#5851=AXIS2_PLACEMENT_3D('',#10545,#7448,#7449);
#5852=AXIS2_PLACEMENT_3D('',#10546,#7450,#7451);
#5853=AXIS2_PLACEMENT_3D('',#10547,#7452,#7453);
#5854=AXIS2_PLACEMENT_3D('',#10548,#7454,#7455);
#5855=AXIS2_PLACEMENT_3D('',#10549,#7456,#7457);
#5856=AXIS2_PLACEMENT_3D('',#10550,#7458,#7459);
#5857=AXIS2_PLACEMENT_3D('',#10551,#7460,#7461);
#5858=AXIS2_PLACEMENT_3D('',#10552,#7462,#7463);
#5859=AXIS2_PLACEMENT_3D('',#10553,#7464,#7465);
#5860=AXIS2_PLACEMENT_3D('',#10554,#7466,#7467);
#5861=AXIS2_PLACEMENT_3D('',#10555,#7468,#7469);
#5862=AXIS2_PLACEMENT_3D('',#10556,#7470,#7471);
#5863=AXIS2_PLACEMENT_3D('',#10557,#7472,#7473);
#5864=AXIS2_PLACEMENT_3D('',#10558,#7474,#7475);
#5865=AXIS2_PLACEMENT_3D('',#10559,#7476,#7477);
#5866=AXIS2_PLACEMENT_3D('',#10560,#7478,#7479);
#5867=AXIS2_PLACEMENT_3D('',#10561,#7480,#7481);
#5868=AXIS2_PLACEMENT_3D('',#10562,#7482,#7483);
#5869=AXIS2_PLACEMENT_3D('',#10563,#7484,#7485);
#5870=DIRECTION('axis',(0.,0.,1.));
#5871=DIRECTION('refdir',(1.,0.,0.));
#5872=DIRECTION('axis',(0.,0.,1.));
#5873=DIRECTION('refdir',(1.,0.,0.));
#5874=DIRECTION('axis',(0.,0.,1.));
#5875=DIRECTION('refdir',(1.,0.,0.));
#5876=DIRECTION('center_axis',(0.,0.,1.));
#5877=DIRECTION('ref_axis',(1.,0.,0.));
#5878=DIRECTION('center_axis',(0.,0.,1.));
#5879=DIRECTION('ref_axis',(1.,0.,0.));
#5880=DIRECTION('',(0.,0.,1.));
#5881=DIRECTION('center_axis',(0.,0.,-1.));
#5882=DIRECTION('ref_axis',(1.,0.,0.));
#5883=DIRECTION('center_axis',(0.,0.,1.));
#5884=DIRECTION('ref_axis',(1.,0.,0.));
#5885=DIRECTION('center_axis',(0.,0.,1.));
#5886=DIRECTION('ref_axis',(1.,0.,0.));
#5887=DIRECTION('',(0.,0.,1.));
#5888=DIRECTION('center_axis',(0.,0.,-1.));
#5889=DIRECTION('ref_axis',(1.,0.,0.));
#5890=DIRECTION('center_axis',(0.,0.,1.));
#5891=DIRECTION('ref_axis',(1.,0.,0.));
#5892=DIRECTION('center_axis',(0.,0.,1.));
#5893=DIRECTION('ref_axis',(1.,0.,0.));
#5894=DIRECTION('',(0.,0.,1.));
#5895=DIRECTION('center_axis',(0.,0.,-1.));
#5896=DIRECTION('ref_axis',(1.,0.,0.));
#5897=DIRECTION('center_axis',(0.,0.,1.));
#5898=DIRECTION('ref_axis',(1.,0.,0.));
#5899=DIRECTION('center_axis',(0.,0.,1.));
#5900=DIRECTION('ref_axis',(1.,0.,0.));
#5901=DIRECTION('',(0.,0.,1.));
#5902=DIRECTION('center_axis',(0.,0.,-1.));
#5903=DIRECTION('ref_axis',(1.,0.,0.));
#5904=DIRECTION('center_axis',(0.,1.,0.));
#5905=DIRECTION('ref_axis',(-1.,0.,0.));
#5906=DIRECTION('',(-1.,0.,0.));
#5907=DIRECTION('',(0.,0.,1.));
#5908=DIRECTION('',(-1.,0.,0.));
#5909=DIRECTION('',(0.,0.,1.));
#5910=DIRECTION('center_axis',(1.,0.,0.));
#5911=DIRECTION('ref_axis',(0.,1.,0.));
#5912=DIRECTION('',(0.,1.,0.));
#5913=DIRECTION('',(0.,1.,0.));
#5914=DIRECTION('',(0.,0.,1.));
#5915=DIRECTION('center_axis',(0.,-1.,0.));
#5916=DIRECTION('ref_axis',(1.,0.,0.));
#5917=DIRECTION('',(1.,0.,0.));
#5918=DIRECTION('',(1.,0.,0.));
#5919=DIRECTION('',(0.,0.,1.));
#5920=DIRECTION('center_axis',(-1.,0.,0.));
#5921=DIRECTION('ref_axis',(0.,-1.,0.));
#5922=DIRECTION('',(0.,-1.,0.));
#5923=DIRECTION('',(0.,-1.,0.));
#5924=DIRECTION('center_axis',(0.,0.,1.));
#5925=DIRECTION('ref_axis',(1.,0.,0.));
#5926=DIRECTION('center_axis',(0.,0.,1.));
#5927=DIRECTION('ref_axis',(1.,0.,0.));
#5928=DIRECTION('axis',(0.,0.,1.));
#5929=DIRECTION('refdir',(1.,0.,0.));
#5930=DIRECTION('center_axis',(0.,1.,0.));
#5931=DIRECTION('ref_axis',(-1.,0.,0.));
#5932=DIRECTION('',(-1.,0.,0.));
#5933=DIRECTION('',(0.,0.,1.));
#5934=DIRECTION('',(-1.,0.,0.));
#5935=DIRECTION('',(0.,0.,1.));
#5936=DIRECTION('center_axis',(1.,0.,0.));
#5937=DIRECTION('ref_axis',(0.,1.,0.));
#5938=DIRECTION('',(0.,1.,0.));
#5939=DIRECTION('',(0.,1.,0.));
#5940=DIRECTION('',(0.,0.,1.));
#5941=DIRECTION('center_axis',(0.,-1.,0.));
#5942=DIRECTION('ref_axis',(1.,0.,0.));
#5943=DIRECTION('',(1.,0.,0.));
#5944=DIRECTION('',(1.,0.,0.));
#5945=DIRECTION('',(0.,0.,1.));
#5946=DIRECTION('center_axis',(-1.,0.,0.));
#5947=DIRECTION('ref_axis',(0.,-1.,0.));
#5948=DIRECTION('',(0.,-1.,0.));
#5949=DIRECTION('',(0.,-1.,0.));
#5950=DIRECTION('center_axis',(0.,0.,1.));
#5951=DIRECTION('ref_axis',(1.,0.,0.));
#5952=DIRECTION('center_axis',(0.,0.,1.));
#5953=DIRECTION('ref_axis',(1.,0.,0.));
#5954=DIRECTION('axis',(0.,0.,1.));
#5955=DIRECTION('refdir',(1.,0.,0.));
#5956=DIRECTION('center_axis',(0.,1.,0.));
#5957=DIRECTION('ref_axis',(-1.,0.,0.));
#5958=DIRECTION('',(-1.,0.,0.));
#5959=DIRECTION('',(0.,0.,1.));
#5960=DIRECTION('',(-1.,0.,0.));
#5961=DIRECTION('',(0.,0.,1.));
#5962=DIRECTION('center_axis',(1.,0.,0.));
#5963=DIRECTION('ref_axis',(0.,1.,0.));
#5964=DIRECTION('',(0.,1.,0.));
#5965=DIRECTION('',(0.,1.,0.));
#5966=DIRECTION('',(0.,0.,1.));
#5967=DIRECTION('center_axis',(0.,-1.,0.));
#5968=DIRECTION('ref_axis',(1.,0.,0.));
#5969=DIRECTION('',(1.,0.,0.));
#5970=DIRECTION('',(1.,0.,0.));
#5971=DIRECTION('',(0.,0.,1.));
#5972=DIRECTION('center_axis',(-1.,0.,0.));
#5973=DIRECTION('ref_axis',(0.,-1.,0.));
#5974=DIRECTION('',(0.,-1.,0.));
#5975=DIRECTION('',(0.,-1.,0.));
#5976=DIRECTION('center_axis',(0.,0.,1.));
#5977=DIRECTION('ref_axis',(1.,0.,0.));
#5978=DIRECTION('center_axis',(0.,0.,1.));
#5979=DIRECTION('ref_axis',(1.,0.,0.));
#5980=DIRECTION('axis',(0.,0.,1.));
#5981=DIRECTION('refdir',(1.,0.,0.));
#5982=DIRECTION('center_axis',(0.,0.,1.));
#5983=DIRECTION('ref_axis',(1.,0.,0.));
#5984=DIRECTION('center_axis',(0.,0.,-1.));
#5985=DIRECTION('ref_axis',(1.,0.,0.));
#5986=DIRECTION('center_axis',(0.,0.,1.));
#5987=DIRECTION('ref_axis',(1.,0.,0.));
#5988=DIRECTION('center_axis',(0.,0.,1.));
#5989=DIRECTION('ref_axis',(1.,0.,0.));
#5990=DIRECTION('center_axis',(0.,0.,1.));
#5991=DIRECTION('ref_axis',(0.707106781186548,0.707106781186547,0.));
#5992=DIRECTION('',(0.,0.,-1.));
#5993=DIRECTION('center_axis',(0.,0.,-1.));
#5994=DIRECTION('ref_axis',(1.,0.,0.));
#5995=DIRECTION('',(0.,0.,1.));
#5996=DIRECTION('center_axis',(0.,0.,1.));
#5997=DIRECTION('ref_axis',(1.,0.,0.));
#5998=DIRECTION('center_axis',(0.,0.,-1.));
#5999=DIRECTION('ref_axis',(1.,0.,0.));
#6000=DIRECTION('center_axis',(0.,0.,1.));
#6001=DIRECTION('ref_axis',(1.,0.,0.));
#6002=DIRECTION('center_axis',(0.,0.,1.));
#6003=DIRECTION('ref_axis',(1.,0.,0.));
#6004=DIRECTION('center_axis',(0.,0.,1.));
#6005=DIRECTION('ref_axis',(0.707106781186547,-0.707106781186548,0.));
#6006=DIRECTION('',(0.,0.,-1.));
#6007=DIRECTION('center_axis',(0.,0.,-1.));
#6008=DIRECTION('ref_axis',(1.,0.,0.));
#6009=DIRECTION('',(0.,0.,1.));
#6010=DIRECTION('center_axis',(0.,0.,1.));
#6011=DIRECTION('ref_axis',(1.,0.,0.));
#6012=DIRECTION('center_axis',(0.,0.,-1.));
#6013=DIRECTION('ref_axis',(1.,0.,0.));
#6014=DIRECTION('center_axis',(0.,0.,1.));
#6015=DIRECTION('ref_axis',(1.,0.,0.));
#6016=DIRECTION('center_axis',(0.,0.,1.));
#6017=DIRECTION('ref_axis',(1.,0.,0.));
#6018=DIRECTION('center_axis',(0.,0.,1.));
#6019=DIRECTION('ref_axis',(-0.707106781186548,-0.707106781186547,0.));
#6020=DIRECTION('',(0.,0.,-1.));
#6021=DIRECTION('center_axis',(0.,0.,-1.));
#6022=DIRECTION('ref_axis',(1.,0.,0.));
#6023=DIRECTION('',(0.,0.,1.));
#6024=DIRECTION('center_axis',(0.,0.,1.));
#6025=DIRECTION('ref_axis',(1.,0.,0.));
#6026=DIRECTION('center_axis',(0.,0.,-1.));
#6027=DIRECTION('ref_axis',(1.,0.,0.));
#6028=DIRECTION('center_axis',(0.,0.,1.));
#6029=DIRECTION('ref_axis',(1.,0.,0.));
#6030=DIRECTION('center_axis',(0.,0.,1.));
#6031=DIRECTION('ref_axis',(1.,0.,0.));
#6032=DIRECTION('center_axis',(0.,0.,1.));
#6033=DIRECTION('ref_axis',(-0.707106781186547,0.707106781186548,0.));
#6034=DIRECTION('',(0.,0.,-1.));
#6035=DIRECTION('center_axis',(0.,0.,-1.));
#6036=DIRECTION('ref_axis',(1.,0.,0.));
#6037=DIRECTION('',(0.,0.,1.));
#6038=DIRECTION('center_axis',(0.,0.,1.));
#6039=DIRECTION('ref_axis',(1.,0.,0.));
#6040=DIRECTION('center_axis',(0.,0.,1.));
#6041=DIRECTION('ref_axis',(1.,0.,0.));
#6042=DIRECTION('center_axis',(0.,0.,1.));
#6043=DIRECTION('ref_axis',(1.,0.,0.));
#6044=DIRECTION('center_axis',(0.,0.,1.));
#6045=DIRECTION('ref_axis',(1.,0.,0.));
#6046=DIRECTION('center_axis',(0.,0.,1.));
#6047=DIRECTION('ref_axis',(1.,0.,0.));
#6048=DIRECTION('center_axis',(0.,0.,1.));
#6049=DIRECTION('ref_axis',(1.,0.,0.));
#6050=DIRECTION('center_axis',(0.,0.,-1.));
#6051=DIRECTION('ref_axis',(1.,0.,0.));
#6052=DIRECTION('center_axis',(0.,0.,1.));
#6053=DIRECTION('ref_axis',(1.,0.,0.));
#6054=DIRECTION('',(0.,0.,-1.));
#6055=DIRECTION('center_axis',(0.,0.,1.));
#6056=DIRECTION('ref_axis',(1.,0.,0.));
#6057=DIRECTION('center_axis',(0.,1.,0.));
#6058=DIRECTION('ref_axis',(1.,0.,0.));
#6059=DIRECTION('center_axis',(0.,1.,0.));
#6060=DIRECTION('ref_axis',(1.,0.,0.));
#6061=DIRECTION('',(0.,-1.,0.));
#6062=DIRECTION('center_axis',(0.,-1.,0.));
#6063=DIRECTION('ref_axis',(1.,0.,0.));
#6064=DIRECTION('center_axis',(0.,1.,0.));
#6065=DIRECTION('ref_axis',(1.,0.,0.));
#6066=DIRECTION('center_axis',(0.,1.,0.));
#6067=DIRECTION('ref_axis',(0.,0.,1.));
#6068=DIRECTION('',(0.,0.,1.));
#6069=DIRECTION('',(-1.,0.,0.));
#6070=DIRECTION('',(0.,0.,-1.));
#6071=DIRECTION('',(-1.,0.,0.));
#6072=DIRECTION('',(0.,0.,1.));
#6073=DIRECTION('',(1.,0.,0.));
#6074=DIRECTION('center_axis',(1.,0.,0.));
#6075=DIRECTION('ref_axis',(0.,0.,-1.));
#6076=DIRECTION('',(0.,1.,0.));
#6077=DIRECTION('',(0.,0.,1.));
#6078=DIRECTION('',(0.,1.,0.));
#6079=DIRECTION('center_axis',(-1.,0.,0.));
#6080=DIRECTION('ref_axis',(0.,0.,1.));
#6081=DIRECTION('',(0.,0.,-1.));
#6082=DIRECTION('',(0.,1.,0.));
#6083=DIRECTION('',(0.,1.,0.));
#6084=DIRECTION('center_axis',(0.,0.,-1.));
#6085=DIRECTION('ref_axis',(-1.,0.,0.));
#6086=DIRECTION('',(1.,0.,0.));
#6087=DIRECTION('center_axis',(-1.,0.,0.));
#6088=DIRECTION('ref_axis',(0.,-1.,0.));
#6089=DIRECTION('',(0.,-1.,0.));
#6090=DIRECTION('',(0.,0.,1.));
#6091=DIRECTION('',(0.,-1.,0.));
#6092=DIRECTION('center_axis',(0.,0.,1.));
#6093=DIRECTION('ref_axis',(1.,0.,0.));
#6094=DIRECTION('',(-1.,0.,0.));
#6095=DIRECTION('',(0.,1.,0.));
#6096=DIRECTION('',(-1.,0.,0.));
#6097=DIRECTION('center_axis',(0.,0.,1.));
#6098=DIRECTION('ref_axis',(1.,0.,0.));
#6099=DIRECTION('',(-1.,0.,0.));
#6100=DIRECTION('center_axis',(0.,1.,0.));
#6101=DIRECTION('ref_axis',(-1.,0.,0.));
#6102=DIRECTION('',(0.,0.,1.));
#6103=DIRECTION('',(-1.,0.,0.));
#6104=DIRECTION('center_axis',(0.,1.,0.));
#6105=DIRECTION('ref_axis',(-1.,0.,0.));
#6106=DIRECTION('',(0.,0.,-1.));
#6107=DIRECTION('',(0.,0.,1.));
#6108=DIRECTION('',(-1.,0.,0.));
#6109=DIRECTION('center_axis',(1.,0.,0.));
#6110=DIRECTION('ref_axis',(0.,1.,0.));
#6111=DIRECTION('',(0.,1.,0.));
#6112=DIRECTION('',(0.,0.,1.));
#6113=DIRECTION('center_axis',(0.,-1.,0.));
#6114=DIRECTION('ref_axis',(1.,0.,0.));
#6115=DIRECTION('',(1.,0.,0.));
#6116=DIRECTION('center_axis',(0.,0.,1.));
#6117=DIRECTION('ref_axis',(1.,0.,0.));
#6118=DIRECTION('center_axis',(0.,0.,-1.));
#6119=DIRECTION('ref_axis',(1.,0.,0.));
#6120=DIRECTION('center_axis',(0.,0.,1.));
#6121=DIRECTION('ref_axis',(1.,0.,0.));
#6122=DIRECTION('',(0.,0.,-1.));
#6123=DIRECTION('center_axis',(0.,0.,-1.));
#6124=DIRECTION('ref_axis',(1.,0.,0.));
#6125=DIRECTION('',(0.,0.,1.));
#6126=DIRECTION('center_axis',(0.,0.,1.));
#6127=DIRECTION('ref_axis',(1.,0.,0.));
#6128=DIRECTION('',(0.,0.,-1.));
#6129=DIRECTION('center_axis',(0.,0.,-1.));
#6130=DIRECTION('ref_axis',(1.,0.,0.));
#6131=DIRECTION('',(0.,0.,-1.));
#6132=DIRECTION('center_axis',(0.,0.,-1.));
#6133=DIRECTION('ref_axis',(1.,0.,0.));
#6134=DIRECTION('',(0.,0.,1.));
#6135=DIRECTION('center_axis',(0.,0.,1.));
#6136=DIRECTION('ref_axis',(1.,0.,0.));
#6137=DIRECTION('center_axis',(0.,1.,0.));
#6138=DIRECTION('ref_axis',(1.,0.,0.));
#6139=DIRECTION('center_axis',(0.,1.,0.));
#6140=DIRECTION('ref_axis',(1.,0.,0.));
#6141=DIRECTION('',(0.,1.,0.));
#6142=DIRECTION('center_axis',(0.,-1.,0.));
#6143=DIRECTION('ref_axis',(1.,0.,0.));
#6144=DIRECTION('center_axis',(0.,0.,1.));
#6145=DIRECTION('ref_axis',(1.,0.,0.));
#6146=DIRECTION('',(0.,1.,0.));
#6147=DIRECTION('',(-1.,0.,0.));
#6148=DIRECTION('',(0.,1.,0.));
#6149=DIRECTION('',(1.,0.,0.));
#6150=DIRECTION('center_axis',(-1.,0.,0.));
#6151=DIRECTION('ref_axis',(0.,0.,1.));
#6152=DIRECTION('',(0.,-1.,0.));
#6153=DIRECTION('',(0.,0.,1.));
#6154=DIRECTION('',(0.,1.,0.));
#6155=DIRECTION('',(0.,0.,-1.));
#6156=DIRECTION('center_axis',(0.,0.,-1.));
#6157=DIRECTION('ref_axis',(-1.,0.,0.));
#6158=DIRECTION('',(1.,0.,0.));
#6159=DIRECTION('',(-1.,0.,0.));
#6160=DIRECTION('',(0.,1.,0.));
#6161=DIRECTION('center_axis',(1.,0.,0.));
#6162=DIRECTION('ref_axis',(0.,0.,-1.));
#6163=DIRECTION('',(0.,0.,1.));
#6164=DIRECTION('',(0.,0.,-1.));
#6165=DIRECTION('center_axis',(0.,1.,0.));
#6166=DIRECTION('ref_axis',(1.,0.,0.));
#6167=DIRECTION('',(1.,0.,0.));
#6168=DIRECTION('',(0.,0.,1.));
#6169=DIRECTION('center_axis',(0.,0.,-1.));
#6170=DIRECTION('ref_axis',(-1.,0.,0.));
#6171=DIRECTION('',(0.,1.,0.));
#6172=DIRECTION('',(1.,0.,0.));
#6173=DIRECTION('',(0.,1.,0.));
#6174=DIRECTION('',(-1.,0.,0.));
#6175=DIRECTION('center_axis',(1.,0.,0.));
#6176=DIRECTION('ref_axis',(0.,0.,-1.));
#6177=DIRECTION('',(0.,0.,-1.));
#6178=DIRECTION('',(0.,1.,0.));
#6179=DIRECTION('',(0.,0.,1.));
#6180=DIRECTION('center_axis',(-1.,0.,0.));
#6181=DIRECTION('ref_axis',(0.,0.,1.));
#6182=DIRECTION('',(0.,1.,0.));
#6183=DIRECTION('',(0.,0.,1.));
#6184=DIRECTION('center_axis',(0.,0.,1.));
#6185=DIRECTION('ref_axis',(1.,0.,0.));
#6186=DIRECTION('',(-1.,0.,0.));
#6187=DIRECTION('',(1.,0.,0.));
#6188=DIRECTION('center_axis',(0.,1.,0.));
#6189=DIRECTION('ref_axis',(0.,0.,1.));
#6190=DIRECTION('center_axis',(0.,1.,0.));
#6191=DIRECTION('ref_axis',(1.,0.,0.));
#6192=DIRECTION('center_axis',(0.,1.,0.));
#6193=DIRECTION('ref_axis',(1.,0.,0.));
#6194=DIRECTION('center_axis',(0.,1.,0.));
#6195=DIRECTION('ref_axis',(1.,0.,0.));
#6196=DIRECTION('',(0.,1.,0.));
#6197=DIRECTION('center_axis',(0.,-1.,0.));
#6198=DIRECTION('ref_axis',(1.,0.,0.));
#6199=DIRECTION('center_axis',(0.,1.,0.));
#6200=DIRECTION('ref_axis',(0.,0.,1.));
#6201=DIRECTION('',(-1.,0.,0.));
#6202=DIRECTION('',(0.,0.,-1.));
#6203=DIRECTION('',(1.,0.,0.));
#6204=DIRECTION('',(0.,0.,-1.));
#6205=DIRECTION('',(-1.,0.,0.));
#6206=DIRECTION('',(0.,0.,1.));
#6207=DIRECTION('center_axis',(0.,0.,1.));
#6208=DIRECTION('ref_axis',(1.,0.,0.));
#6209=DIRECTION('',(0.,1.,0.));
#6210=DIRECTION('',(-1.,0.,0.));
#6211=DIRECTION('',(0.,1.,0.));
#6212=DIRECTION('center_axis',(-1.,0.,0.));
#6213=DIRECTION('ref_axis',(0.,0.,1.));
#6214=DIRECTION('',(0.,-1.,0.));
#6215=DIRECTION('',(0.,1.,0.));
#6216=DIRECTION('',(0.,0.,-1.));
#6217=DIRECTION('center_axis',(0.,0.,-1.));
#6218=DIRECTION('ref_axis',(-1.,0.,0.));
#6219=DIRECTION('',(1.,0.,0.));
#6220=DIRECTION('',(0.,1.,0.));
#6221=DIRECTION('center_axis',(1.,0.,0.));
#6222=DIRECTION('ref_axis',(0.,0.,-1.));
#6223=DIRECTION('',(0.,0.,1.));
#6224=DIRECTION('center_axis',(0.,1.,0.));
#6225=DIRECTION('ref_axis',(1.,0.,0.));
#6226=DIRECTION('',(0.,0.,1.));
#6227=DIRECTION('',(-1.,0.,0.));
#6228=DIRECTION('',(0.,0.,-1.));
#6229=DIRECTION('',(1.,0.,0.));
#6230=DIRECTION('center_axis',(0.,0.,1.));
#6231=DIRECTION('ref_axis',(1.,0.,0.));
#6232=DIRECTION('',(0.,1.,0.));
#6233=DIRECTION('',(0.,1.,0.));
#6234=DIRECTION('',(1.,0.,0.));
#6235=DIRECTION('center_axis',(-1.,0.,0.));
#6236=DIRECTION('ref_axis',(0.,0.,1.));
#6237=DIRECTION('',(0.,1.,0.));
#6238=DIRECTION('center_axis',(0.,0.,-1.));
#6239=DIRECTION('ref_axis',(-1.,0.,0.));
#6240=DIRECTION('',(-1.,0.,0.));
#6241=DIRECTION('',(0.,1.,0.));
#6242=DIRECTION('center_axis',(1.,0.,0.));
#6243=DIRECTION('ref_axis',(0.,0.,-1.));
#6244=DIRECTION('',(0.,0.,-1.));
#6245=DIRECTION('center_axis',(0.,1.,0.));
#6246=DIRECTION('ref_axis',(0.,0.,1.));
#6247=DIRECTION('center_axis',(0.,0.,1.));
#6248=DIRECTION('ref_axis',(1.,0.,0.));
#6249=DIRECTION('center_axis',(0.,0.,1.));
#6250=DIRECTION('ref_axis',(1.,0.,0.));
#6251=DIRECTION('',(0.,0.,1.));
#6252=DIRECTION('center_axis',(0.,0.,1.));
#6253=DIRECTION('ref_axis',(1.,0.,0.));
#6254=DIRECTION('center_axis',(0.,0.,1.));
#6255=DIRECTION('ref_axis',(1.,0.,0.));
#6256=DIRECTION('',(0.,0.,1.));
#6257=DIRECTION('center_axis',(0.,0.,1.));
#6258=DIRECTION('ref_axis',(1.,0.,0.));
#6259=DIRECTION('center_axis',(0.,0.,1.));
#6260=DIRECTION('ref_axis',(1.,0.,0.));
#6261=DIRECTION('',(0.,0.,1.));
#6262=DIRECTION('center_axis',(0.,0.,1.));
#6263=DIRECTION('ref_axis',(1.,0.,0.));
#6264=DIRECTION('center_axis',(0.,0.,1.));
#6265=DIRECTION('ref_axis',(1.,0.,0.));
#6266=DIRECTION('',(0.,0.,1.));
#6267=DIRECTION('center_axis',(0.,0.,1.));
#6268=DIRECTION('ref_axis',(1.,0.,0.));
#6269=DIRECTION('center_axis',(0.,0.,1.));
#6270=DIRECTION('ref_axis',(1.,0.,0.));
#6271=DIRECTION('center_axis',(0.,0.,1.));
#6272=DIRECTION('ref_axis',(1.,0.,0.));
#6273=DIRECTION('center_axis',(0.,0.,1.));
#6274=DIRECTION('ref_axis',(1.,0.,0.));
#6275=DIRECTION('center_axis',(0.,0.,1.));
#6276=DIRECTION('ref_axis',(1.,0.,0.));
#6277=DIRECTION('',(0.,0.,-1.));
#6278=DIRECTION('center_axis',(0.,0.,1.));
#6279=DIRECTION('ref_axis',(1.,0.,0.));
#6280=DIRECTION('center_axis',(0.,0.,1.));
#6281=DIRECTION('ref_axis',(1.,0.,0.));
#6282=DIRECTION('',(0.,0.,-1.));
#6283=DIRECTION('center_axis',(0.,0.,1.));
#6284=DIRECTION('ref_axis',(1.,0.,0.));
#6285=DIRECTION('axis',(0.,0.,1.));
#6286=DIRECTION('refdir',(1.,0.,0.));
#6287=DIRECTION('center_axis',(0.,1.,0.));
#6288=DIRECTION('ref_axis',(-1.,0.,0.));
#6289=DIRECTION('',(-1.,0.,0.));
#6290=DIRECTION('',(0.,0.,1.));
#6291=DIRECTION('',(-1.,0.,0.));
#6292=DIRECTION('',(0.,0.,1.));
#6293=DIRECTION('center_axis',(1.,0.,0.));
#6294=DIRECTION('ref_axis',(0.,1.,0.));
#6295=DIRECTION('',(0.,1.,0.));
#6296=DIRECTION('',(0.,1.,0.));
#6297=DIRECTION('',(0.,0.,1.));
#6298=DIRECTION('center_axis',(0.,-1.,0.));
#6299=DIRECTION('ref_axis',(1.,0.,0.));
#6300=DIRECTION('',(1.,0.,0.));
#6301=DIRECTION('',(1.,0.,0.));
#6302=DIRECTION('',(0.,0.,1.));
#6303=DIRECTION('center_axis',(-1.,0.,0.));
#6304=DIRECTION('ref_axis',(0.,-1.,0.));
#6305=DIRECTION('',(0.,-1.,0.));
#6306=DIRECTION('',(0.,-1.,0.));
#6307=DIRECTION('center_axis',(0.,0.,1.));
#6308=DIRECTION('ref_axis',(1.,0.,0.));
#6309=DIRECTION('center_axis',(0.,0.,1.));
#6310=DIRECTION('ref_axis',(1.,0.,0.));
#6311=DIRECTION('axis',(0.,0.,1.));
#6312=DIRECTION('refdir',(1.,0.,0.));
#6313=DIRECTION('center_axis',(-0.000134431341915714,0.998590099522227,
0.0530829074599677));
#6314=DIRECTION('ref_axis',(7.14608168190195E-6,-0.0530829069789608,0.998590108570877));
#6315=DIRECTION('center_axis',(0.000134431323893231,0.998590099521685,0.0530829074702145));
#6316=DIRECTION('ref_axis',(0.202244098525442,0.0519588076800388,-0.977955830759294));
#6317=DIRECTION('center_axis',(0.000134431323893231,0.998590099521685,0.0530829074702145));
#6318=DIRECTION('ref_axis',(0.202244098525442,0.0519588076800388,-0.977955830759294));
#6319=DIRECTION('center_axis',(-0.000134431341915714,0.998590099522227,
0.0530829074599677));
#6320=DIRECTION('ref_axis',(7.14608168190194E-6,-0.0530829069789608,0.998590108570877));
#6321=DIRECTION('axis',(0.,0.,1.));
#6322=DIRECTION('refdir',(1.,0.,0.));
#6323=DIRECTION('center_axis',(0.866025403784439,0.,-0.5));
#6324=DIRECTION('ref_axis',(0.5,0.,0.866025403784439));
#6325=DIRECTION('',(-0.5,0.,-0.866025403784439));
#6326=DIRECTION('',(0.,-1.,0.));
#6327=DIRECTION('',(0.5,0.,0.866025403784439));
#6328=DIRECTION('',(0.,-1.,0.));
#6329=DIRECTION('center_axis',(1.20185167898973E-16,0.,-1.));
#6330=DIRECTION('ref_axis',(1.,0.,1.20185167898973E-16));
#6331=DIRECTION('',(-1.,0.,-1.20185167898973E-16));
#6332=DIRECTION('',(0.,-1.,0.));
#6333=DIRECTION('',(1.,0.,1.20185167898973E-16));
#6334=DIRECTION('center_axis',(-0.866025403784439,0.,-0.5));
#6335=DIRECTION('ref_axis',(0.5,0.,-0.866025403784439));
#6336=DIRECTION('',(-0.5,0.,0.866025403784439));
#6337=DIRECTION('',(0.,-1.,0.));
#6338=DIRECTION('',(0.5,0.,-0.866025403784439));
#6339=DIRECTION('center_axis',(-0.866025403784439,0.,0.5));
#6340=DIRECTION('ref_axis',(-0.5,0.,-0.866025403784439));
#6341=DIRECTION('',(0.5,0.,0.866025403784439));
#6342=DIRECTION('',(0.,-1.,0.));
#6343=DIRECTION('',(-0.5,0.,-0.866025403784439));
#6344=DIRECTION('center_axis',(-2.40370335797945E-16,0.,1.));
#6345=DIRECTION('ref_axis',(-1.,0.,-2.40370335797945E-16));
#6346=DIRECTION('',(1.,0.,2.40370335797945E-16));
#6347=DIRECTION('',(0.,-1.,0.));
#6348=DIRECTION('',(-1.,0.,-2.40370335797945E-16));
#6349=DIRECTION('center_axis',(0.866025403784439,0.,0.5));
#6350=DIRECTION('ref_axis',(-0.5,0.,0.866025403784439));
#6351=DIRECTION('',(0.5,0.,-0.866025403784439));
#6352=DIRECTION('',(-0.5,0.,0.866025403784439));
#6353=DIRECTION('center_axis',(0.,1.,0.));
#6354=DIRECTION('ref_axis',(1.,0.,0.));
#6355=DIRECTION('center_axis',(0.,-1.,0.));
#6356=DIRECTION('ref_axis',(0.,0.,-1.));
#6357=DIRECTION('center_axis',(0.,1.,0.));
#6358=DIRECTION('ref_axis',(1.,0.,0.));
#6359=DIRECTION('center_axis',(0.,1.,0.));
#6360=DIRECTION('ref_axis',(1.,0.,0.));
#6361=DIRECTION('center_axis',(0.,1.,0.));
#6362=DIRECTION('ref_axis',(0.,0.,1.));
#6363=DIRECTION('center_axis',(0.,-1.,0.));
#6364=DIRECTION('ref_axis',(1.,0.,0.));
#6365=DIRECTION('center_axis',(0.,-1.,0.));
#6366=DIRECTION('ref_axis',(1.,0.,0.));
#6367=DIRECTION('center_axis',(0.,-1.,0.));
#6368=DIRECTION('ref_axis',(1.,0.,0.));
#6369=DIRECTION('',(0.707106781186548,0.707106781186547,8.65956056235493E-17));
#6370=DIRECTION('center_axis',(0.,-1.,0.));
#6371=DIRECTION('ref_axis',(1.,0.,0.));
#6372=DIRECTION('center_axis',(0.,-1.,0.));
#6373=DIRECTION('ref_axis',(1.,0.,0.));
#6374=DIRECTION('',(0.,1.,0.));
#6375=DIRECTION('center_axis',(0.,1.,0.));
#6376=DIRECTION('ref_axis',(1.,0.,0.));
#6377=DIRECTION('center_axis',(0.,-1.,0.));
#6378=DIRECTION('ref_axis',(1.,0.,0.));
#6379=DIRECTION('',(-0.707106781186547,0.707106781186548,-8.65956056235493E-17));
#6380=DIRECTION('center_axis',(0.,-1.,0.));
#6381=DIRECTION('ref_axis',(0.,0.,-1.));
#6382=DIRECTION('center_axis',(0.,-1.,0.));
#6383=DIRECTION('ref_axis',(1.,0.,0.));
#6384=DIRECTION('center_axis',(0.,1.,0.));
#6385=DIRECTION('ref_axis',(1.,0.,0.));
#6386=DIRECTION('center_axis',(0.,1.,0.));
#6387=DIRECTION('ref_axis',(1.,0.,0.));
#6388=DIRECTION('',(-0.447213595499958,0.894427190999916,-5.47678698264203E-17));
#6389=DIRECTION('center_axis',(0.,-1.,0.));
#6390=DIRECTION('ref_axis',(1.,0.,0.));
#6391=DIRECTION('',(0.,1.,0.));
#6392=DIRECTION('',(0.,0.,1.));
#6393=DIRECTION('',(1.,0.,0.));
#6394=DIRECTION('',(0.,0.,1.));
#6395=DIRECTION('',(1.,0.,0.));
#6396=DIRECTION('',(0.,0.,1.));
#6397=DIRECTION('',(1.,0.,0.));
#6398=DIRECTION('',(0.,0.,1.));
#6399=DIRECTION('',(1.,0.,0.));
#6400=DIRECTION('',(0.,0.,1.));
#6401=DIRECTION('',(1.,0.,0.));
#6402=DIRECTION('',(0.,0.,1.));
#6403=DIRECTION('',(1.,0.,0.));
#6404=DIRECTION('',(0.,-1.,2.22044604925031E-16));
#6405=DIRECTION('',(1.,0.,0.));
#6406=DIRECTION('',(0.,-1.,2.22044604925031E-16));
#6407=DIRECTION('',(1.,0.,0.));
#6408=DIRECTION('',(0.,-1.,2.22044604925031E-16));
#6409=DIRECTION('',(1.,0.,0.));
#6410=DIRECTION('',(0.,-1.,2.22044604925031E-16));
#6411=DIRECTION('',(1.,0.,0.));
#6412=DIRECTION('axis',(0.,0.,1.));
#6413=DIRECTION('refdir',(1.,0.,0.));
#6414=DIRECTION('axis',(0.,0.,1.));
#6415=DIRECTION('refdir',(1.,0.,0.));
#6416=DIRECTION('center_axis',(0.,0.,1.));
#6417=DIRECTION('ref_axis',(1.,0.,0.));
#6418=DIRECTION('center_axis',(0.,0.,1.));
#6419=DIRECTION('ref_axis',(1.,0.,0.));
#6420=DIRECTION('',(0.,0.,1.));
#6421=DIRECTION('center_axis',(0.,0.,-1.));
#6422=DIRECTION('ref_axis',(1.,0.,0.));
#6423=DIRECTION('center_axis',(0.,0.,1.));
#6424=DIRECTION('ref_axis',(1.,0.,0.));
#6425=DIRECTION('center_axis',(0.,0.,1.));
#6426=DIRECTION('ref_axis',(1.,0.,0.));
#6427=DIRECTION('center_axis',(0.,0.,1.));
#6428=DIRECTION('ref_axis',(1.,0.,0.));
#6429=DIRECTION('',(0.,0.,1.));
#6430=DIRECTION('center_axis',(0.,0.,-1.));
#6431=DIRECTION('ref_axis',(1.,0.,0.));
#6432=DIRECTION('center_axis',(0.,0.,1.));
#6433=DIRECTION('ref_axis',(1.,0.,0.));
#6434=DIRECTION('center_axis',(0.,0.,1.));
#6435=DIRECTION('ref_axis',(1.,0.,0.));
#6436=DIRECTION('center_axis',(0.,0.,1.));
#6437=DIRECTION('ref_axis',(1.,0.,0.));
#6438=DIRECTION('',(0.,0.,1.));
#6439=DIRECTION('center_axis',(0.,0.,-1.));
#6440=DIRECTION('ref_axis',(1.,0.,0.));
#6441=DIRECTION('center_axis',(0.,0.,1.));
#6442=DIRECTION('ref_axis',(1.,0.,0.));
#6443=DIRECTION('center_axis',(0.,0.,1.));
#6444=DIRECTION('ref_axis',(1.,0.,0.));
#6445=DIRECTION('center_axis',(0.,0.,1.));
#6446=DIRECTION('ref_axis',(1.,0.,0.));
#6447=DIRECTION('',(0.,0.,1.));
#6448=DIRECTION('center_axis',(0.,0.,-1.));
#6449=DIRECTION('ref_axis',(1.,0.,0.));
#6450=DIRECTION('center_axis',(0.,0.,1.));
#6451=DIRECTION('ref_axis',(1.,0.,0.));
#6452=DIRECTION('center_axis',(0.,0.,1.));
#6453=DIRECTION('ref_axis',(1.,0.,0.));
#6454=DIRECTION('center_axis',(0.,0.,1.));
#6455=DIRECTION('ref_axis',(1.,0.,0.));
#6456=DIRECTION('',(0.,0.,1.));
#6457=DIRECTION('center_axis',(0.,0.,1.));
#6458=DIRECTION('ref_axis',(1.,0.,0.));
#6459=DIRECTION('center_axis',(0.,0.,1.));
#6460=DIRECTION('ref_axis',(1.,0.,0.));
#6461=DIRECTION('center_axis',(0.,0.,1.));
#6462=DIRECTION('ref_axis',(1.,0.,0.));
#6463=DIRECTION('center_axis',(0.,0.,1.));
#6464=DIRECTION('ref_axis',(1.,0.,0.));
#6465=DIRECTION('',(0.,0.,1.));
#6466=DIRECTION('center_axis',(0.,0.,1.));
#6467=DIRECTION('ref_axis',(1.,0.,0.));
#6468=DIRECTION('center_axis',(0.,0.,1.));
#6469=DIRECTION('ref_axis',(1.,0.,0.));
#6470=DIRECTION('center_axis',(0.,0.,1.));
#6471=DIRECTION('ref_axis',(1.,0.,0.));
#6472=DIRECTION('center_axis',(0.,0.,1.));
#6473=DIRECTION('ref_axis',(1.,0.,0.));
#6474=DIRECTION('',(0.,0.,1.));
#6475=DIRECTION('center_axis',(0.,0.,1.));
#6476=DIRECTION('ref_axis',(1.,0.,0.));
#6477=DIRECTION('center_axis',(0.,0.,1.));
#6478=DIRECTION('ref_axis',(1.,0.,0.));
#6479=DIRECTION('center_axis',(0.,0.,1.));
#6480=DIRECTION('ref_axis',(1.,0.,0.));
#6481=DIRECTION('center_axis',(0.,0.,1.));
#6482=DIRECTION('ref_axis',(1.,0.,0.));
#6483=DIRECTION('',(0.,0.,1.));
#6484=DIRECTION('center_axis',(0.,0.,1.));
#6485=DIRECTION('ref_axis',(1.,0.,0.));
#6486=DIRECTION('center_axis',(0.,0.,1.));
#6487=DIRECTION('ref_axis',(1.,0.,0.));
#6488=DIRECTION('center_axis',(0.,0.,1.));
#6489=DIRECTION('ref_axis',(1.,0.,0.));
#6490=DIRECTION('center_axis',(0.,0.,1.));
#6491=DIRECTION('ref_axis',(1.,0.,0.));
#6492=DIRECTION('',(0.,0.,1.));
#6493=DIRECTION('center_axis',(0.,0.,1.));
#6494=DIRECTION('ref_axis',(1.,0.,0.));
#6495=DIRECTION('center_axis',(0.,0.,1.));
#6496=DIRECTION('ref_axis',(1.,0.,0.));
#6497=DIRECTION('center_axis',(0.,0.,1.));
#6498=DIRECTION('ref_axis',(1.,0.,0.));
#6499=DIRECTION('',(0.,0.,-1.));
#6500=DIRECTION('center_axis',(0.,0.,1.));
#6501=DIRECTION('ref_axis',(1.,0.,0.));
#6502=DIRECTION('',(0.,0.,1.));
#6503=DIRECTION('center_axis',(0.,0.,1.));
#6504=DIRECTION('ref_axis',(1.,0.,0.));
#6505=DIRECTION('center_axis',(0.,0.,1.));
#6506=DIRECTION('ref_axis',(1.,0.,0.));
#6507=DIRECTION('',(1.,0.,0.));
#6508=DIRECTION('center_axis',(0.,0.,-1.));
#6509=DIRECTION('ref_axis',(1.,0.,0.));
#6510=DIRECTION('',(-1.,0.,0.));
#6511=DIRECTION('center_axis',(0.,-1.,0.));
#6512=DIRECTION('ref_axis',(1.,0.,0.));
#6513=DIRECTION('',(1.,0.,0.));
#6514=DIRECTION('',(0.,0.,1.));
#6515=DIRECTION('center_axis',(0.,1.,0.));
#6516=DIRECTION('ref_axis',(-1.,0.,0.));
#6517=DIRECTION('',(0.,0.,-1.));
#6518=DIRECTION('',(-1.,0.,0.));
#6519=DIRECTION('center_axis',(0.,0.,1.));
#6520=DIRECTION('ref_axis',(1.,0.,0.));
#6521=DIRECTION('center_axis',(0.,0.,1.));
#6522=DIRECTION('ref_axis',(1.,0.,0.));
#6523=DIRECTION('center_axis',(0.,0.,1.));
#6524=DIRECTION('ref_axis',(1.,0.,0.));
#6525=DIRECTION('center_axis',(0.,0.,-1.));
#6526=DIRECTION('ref_axis',(1.,0.,0.));
#6527=DIRECTION('',(0.,0.,-1.));
#6528=DIRECTION('center_axis',(0.,0.,-1.));
#6529=DIRECTION('ref_axis',(1.,0.,0.));
#6530=DIRECTION('center_axis',(0.,0.,1.));
#6531=DIRECTION('ref_axis',(1.,0.,0.));
#6532=DIRECTION('center_axis',(0.,0.,1.));
#6533=DIRECTION('ref_axis',(1.,0.,0.));
#6534=DIRECTION('',(0.,0.,-1.));
#6535=DIRECTION('center_axis',(0.,0.,1.));
#6536=DIRECTION('ref_axis',(1.,0.,0.));
#6537=DIRECTION('center_axis',(0.,0.,1.));
#6538=DIRECTION('ref_axis',(1.,0.,0.));
#6539=DIRECTION('center_axis',(0.,0.,1.));
#6540=DIRECTION('ref_axis',(1.,0.,0.));
#6541=DIRECTION('axis',(0.,0.,1.));
#6542=DIRECTION('refdir',(1.,0.,0.));
#6543=DIRECTION('center_axis',(0.,0.,1.));
#6544=DIRECTION('ref_axis',(1.,0.,0.));
#6545=DIRECTION('center_axis',(0.,0.,-1.));
#6546=DIRECTION('ref_axis',(1.,0.,0.));
#6547=DIRECTION('',(0.,0.,-1.));
#6548=DIRECTION('center_axis',(0.,0.,-1.));
#6549=DIRECTION('ref_axis',(1.,0.,0.));
#6550=DIRECTION('center_axis',(0.,0.,1.));
#6551=DIRECTION('ref_axis',(1.,0.,0.));
#6552=DIRECTION('center_axis',(0.,0.,1.));
#6553=DIRECTION('ref_axis',(1.,0.,0.));
#6554=DIRECTION('',(0.,0.,-1.));
#6555=DIRECTION('center_axis',(0.,0.,1.));
#6556=DIRECTION('ref_axis',(1.,0.,0.));
#6557=DIRECTION('center_axis',(0.,0.,1.));
#6558=DIRECTION('ref_axis',(1.,0.,0.));
#6559=DIRECTION('center_axis',(0.,0.,1.));
#6560=DIRECTION('ref_axis',(1.,0.,0.));
#6561=DIRECTION('axis',(0.,0.,1.));
#6562=DIRECTION('refdir',(1.,0.,0.));
#6563=DIRECTION('center_axis',(0.,0.,1.));
#6564=DIRECTION('ref_axis',(1.,0.,0.));
#6565=DIRECTION('center_axis',(0.,0.,-1.));
#6566=DIRECTION('ref_axis',(1.,0.,0.));
#6567=DIRECTION('',(0.,0.,-1.));
#6568=DIRECTION('center_axis',(0.,0.,-1.));
#6569=DIRECTION('ref_axis',(1.,0.,0.));
#6570=DIRECTION('center_axis',(0.,0.,1.));
#6571=DIRECTION('ref_axis',(1.,0.,0.));
#6572=DIRECTION('center_axis',(0.,0.,1.));
#6573=DIRECTION('ref_axis',(1.,0.,0.));
#6574=DIRECTION('',(0.,0.,-1.));
#6575=DIRECTION('center_axis',(0.,0.,1.));
#6576=DIRECTION('ref_axis',(1.,0.,0.));
#6577=DIRECTION('center_axis',(0.,0.,1.));
#6578=DIRECTION('ref_axis',(1.,0.,0.));
#6579=DIRECTION('center_axis',(0.,0.,1.));
#6580=DIRECTION('ref_axis',(1.,0.,0.));
#6581=DIRECTION('axis',(0.,0.,1.));
#6582=DIRECTION('refdir',(1.,0.,0.));
#6583=DIRECTION('center_axis',(0.,0.,1.));
#6584=DIRECTION('ref_axis',(1.,0.,0.));
#6585=DIRECTION('center_axis',(0.,0.,1.));
#6586=DIRECTION('ref_axis',(1.,0.,0.));
#6587=DIRECTION('',(0.,0.,1.));
#6588=DIRECTION('center_axis',(0.,0.,1.));
#6589=DIRECTION('ref_axis',(1.,0.,0.));
#6590=DIRECTION('center_axis',(0.,0.,1.));
#6591=DIRECTION('ref_axis',(1.,0.,0.));
#6592=DIRECTION('center_axis',(0.,0.,-1.));
#6593=DIRECTION('ref_axis',(1.,0.,0.));
#6594=DIRECTION('center_axis',(0.,0.,1.));
#6595=DIRECTION('ref_axis',(1.,0.,0.));
#6596=DIRECTION('center_axis',(0.,0.,1.));
#6597=DIRECTION('ref_axis',(1.,0.,0.));
#6598=DIRECTION('',(0.,0.,1.));
#6599=DIRECTION('center_axis',(0.,0.,1.));
#6600=DIRECTION('ref_axis',(1.,0.,0.));
#6601=DIRECTION('center_axis',(0.,0.,1.));
#6602=DIRECTION('ref_axis',(1.,0.,0.));
#6603=DIRECTION('center_axis',(0.,0.,-1.));
#6604=DIRECTION('ref_axis',(1.,0.,0.));
#6605=DIRECTION('center_axis',(0.,0.,1.));
#6606=DIRECTION('ref_axis',(1.,0.,0.));
#6607=DIRECTION('center_axis',(0.,0.,1.));
#6608=DIRECTION('ref_axis',(1.,0.,0.));
#6609=DIRECTION('',(0.,0.,1.));
#6610=DIRECTION('center_axis',(0.,0.,1.));
#6611=DIRECTION('ref_axis',(1.,0.,0.));
#6612=DIRECTION('center_axis',(0.,0.,1.));
#6613=DIRECTION('ref_axis',(1.,0.,0.));
#6614=DIRECTION('center_axis',(0.,0.,-1.));
#6615=DIRECTION('ref_axis',(1.,0.,0.));
#6616=DIRECTION('center_axis',(0.,0.,1.));
#6617=DIRECTION('ref_axis',(1.,0.,0.));
#6618=DIRECTION('center_axis',(0.,0.,1.));
#6619=DIRECTION('ref_axis',(1.,0.,0.));
#6620=DIRECTION('',(0.,0.,1.));
#6621=DIRECTION('center_axis',(0.,0.,1.));
#6622=DIRECTION('ref_axis',(1.,0.,0.));
#6623=DIRECTION('center_axis',(0.,0.,1.));
#6624=DIRECTION('ref_axis',(1.,0.,0.));
#6625=DIRECTION('center_axis',(0.,0.,-1.));
#6626=DIRECTION('ref_axis',(1.,0.,0.));
#6627=DIRECTION('center_axis',(0.,0.,1.));
#6628=DIRECTION('ref_axis',(1.,0.,0.));
#6629=DIRECTION('',(0.,0.,1.));
#6630=DIRECTION('center_axis',(0.,0.,-1.));
#6631=DIRECTION('ref_axis',(1.,0.,0.));
#6632=DIRECTION('center_axis',(0.,0.,1.));
#6633=DIRECTION('ref_axis',(1.,0.,0.));
#6634=DIRECTION('',(0.,0.,1.));
#6635=DIRECTION('center_axis',(0.,0.,-1.));
#6636=DIRECTION('ref_axis',(1.,0.,0.));
#6637=DIRECTION('center_axis',(0.,0.,1.));
#6638=DIRECTION('ref_axis',(1.,0.,0.));
#6639=DIRECTION('',(0.,0.,1.));
#6640=DIRECTION('center_axis',(0.,0.,-1.));
#6641=DIRECTION('ref_axis',(1.,0.,0.));
#6642=DIRECTION('center_axis',(0.,0.,1.));
#6643=DIRECTION('ref_axis',(1.,0.,0.));
#6644=DIRECTION('',(0.,0.,1.));
#6645=DIRECTION('center_axis',(0.,0.,-1.));
#6646=DIRECTION('ref_axis',(1.,0.,0.));
#6647=DIRECTION('center_axis',(0.,0.,1.));
#6648=DIRECTION('ref_axis',(1.,0.,0.));
#6649=DIRECTION('center_axis',(0.,0.,1.));
#6650=DIRECTION('ref_axis',(1.,0.,0.));
#6651=DIRECTION('',(0.,0.,-1.));
#6652=DIRECTION('center_axis',(0.,0.,-1.));
#6653=DIRECTION('ref_axis',(1.,0.,0.));
#6654=DIRECTION('center_axis',(0.,0.,1.));
#6655=DIRECTION('ref_axis',(1.,0.,0.));
#6656=DIRECTION('center_axis',(0.,0.,-1.));
#6657=DIRECTION('ref_axis',(1.,0.,0.));
#6658=DIRECTION('center_axis',(0.,0.,1.));
#6659=DIRECTION('ref_axis',(1.,0.,0.));
#6660=DIRECTION('',(0.,0.,-1.));
#6661=DIRECTION('center_axis',(0.,0.,-1.));
#6662=DIRECTION('ref_axis',(1.,0.,0.));
#6663=DIRECTION('center_axis',(0.,0.,1.));
#6664=DIRECTION('ref_axis',(1.,0.,0.));
#6665=DIRECTION('center_axis',(0.,0.,1.));
#6666=DIRECTION('ref_axis',(1.,0.,0.));
#6667=DIRECTION('',(0.,0.,-1.));
#6668=DIRECTION('center_axis',(0.,0.,1.));
#6669=DIRECTION('ref_axis',(1.,0.,0.));
#6670=DIRECTION('center_axis',(0.,0.,1.));
#6671=DIRECTION('ref_axis',(1.,0.,0.));
#6672=DIRECTION('center_axis',(0.,0.,1.));
#6673=DIRECTION('ref_axis',(1.,0.,0.));
#6674=DIRECTION('axis',(0.,0.,1.));
#6675=DIRECTION('refdir',(1.,0.,0.));
#6676=DIRECTION('center_axis',(0.,0.,1.));
#6677=DIRECTION('ref_axis',(1.,0.,0.));
#6678=DIRECTION('center_axis',(0.,0.,1.));
#6679=DIRECTION('ref_axis',(1.,0.,0.));
#6680=DIRECTION('',(0.,0.,1.));
#6681=DIRECTION('center_axis',(0.,0.,-1.));
#6682=DIRECTION('ref_axis',(1.,0.,0.));
#6683=DIRECTION('center_axis',(0.,0.,1.));
#6684=DIRECTION('ref_axis',(1.,0.,0.));
#6685=DIRECTION('center_axis',(0.,0.,1.));
#6686=DIRECTION('ref_axis',(1.,0.,0.));
#6687=DIRECTION('center_axis',(0.,0.,1.));
#6688=DIRECTION('ref_axis',(1.,0.,0.));
#6689=DIRECTION('center_axis',(0.,0.,1.));
#6690=DIRECTION('ref_axis',(1.,0.,0.));
#6691=DIRECTION('',(0.,0.,1.));
#6692=DIRECTION('center_axis',(0.,0.,-1.));
#6693=DIRECTION('ref_axis',(1.,0.,0.));
#6694=DIRECTION('center_axis',(0.,0.,1.));
#6695=DIRECTION('ref_axis',(1.,0.,0.));
#6696=DIRECTION('center_axis',(0.,0.,1.));
#6697=DIRECTION('ref_axis',(1.,0.,0.));
#6698=DIRECTION('center_axis',(0.,0.,1.));
#6699=DIRECTION('ref_axis',(1.,0.,0.));
#6700=DIRECTION('center_axis',(0.,0.,1.));
#6701=DIRECTION('ref_axis',(1.,0.,0.));
#6702=DIRECTION('',(0.,0.,1.));
#6703=DIRECTION('center_axis',(0.,0.,-1.));
#6704=DIRECTION('ref_axis',(1.,0.,0.));
#6705=DIRECTION('center_axis',(0.,0.,1.));
#6706=DIRECTION('ref_axis',(1.,0.,0.));
#6707=DIRECTION('center_axis',(0.,0.,1.));
#6708=DIRECTION('ref_axis',(1.,0.,0.));
#6709=DIRECTION('center_axis',(0.,0.,1.));
#6710=DIRECTION('ref_axis',(1.,0.,0.));
#6711=DIRECTION('center_axis',(0.,0.,1.));
#6712=DIRECTION('ref_axis',(1.,0.,0.));
#6713=DIRECTION('',(0.,0.,1.));
#6714=DIRECTION('center_axis',(0.,0.,-1.));
#6715=DIRECTION('ref_axis',(1.,0.,0.));
#6716=DIRECTION('center_axis',(0.,0.,1.));
#6717=DIRECTION('ref_axis',(1.,0.,0.));
#6718=DIRECTION('center_axis',(0.,0.,1.));
#6719=DIRECTION('ref_axis',(1.,0.,0.));
#6720=DIRECTION('center_axis',(0.,0.,1.));
#6721=DIRECTION('ref_axis',(1.,0.,0.));
#6722=DIRECTION('center_axis',(0.,0.,1.));
#6723=DIRECTION('ref_axis',(1.,0.,0.));
#6724=DIRECTION('',(0.,0.,1.));
#6725=DIRECTION('center_axis',(0.,0.,1.));
#6726=DIRECTION('ref_axis',(1.,0.,0.));
#6727=DIRECTION('center_axis',(0.,0.,1.));
#6728=DIRECTION('ref_axis',(1.,0.,0.));
#6729=DIRECTION('',(0.,0.,1.));
#6730=DIRECTION('center_axis',(0.,0.,1.));
#6731=DIRECTION('ref_axis',(1.,0.,0.));
#6732=DIRECTION('center_axis',(0.,0.,1.));
#6733=DIRECTION('ref_axis',(1.,0.,0.));
#6734=DIRECTION('',(0.,0.,1.));
#6735=DIRECTION('center_axis',(0.,0.,1.));
#6736=DIRECTION('ref_axis',(1.,0.,0.));
#6737=DIRECTION('center_axis',(0.,0.,1.));
#6738=DIRECTION('ref_axis',(1.,0.,0.));
#6739=DIRECTION('',(0.,0.,1.));
#6740=DIRECTION('center_axis',(0.,1.,0.));
#6741=DIRECTION('ref_axis',(-1.,0.,0.));
#6742=DIRECTION('',(0.,0.,-1.));
#6743=DIRECTION('',(-1.,0.,0.));
#6744=DIRECTION('',(0.,0.,1.));
#6745=DIRECTION('',(-1.,0.,0.));
#6746=DIRECTION('center_axis',(0.,-1.,0.));
#6747=DIRECTION('ref_axis',(1.,0.,0.));
#6748=DIRECTION('',(0.,0.,1.));
#6749=DIRECTION('',(1.,0.,0.));
#6750=DIRECTION('',(0.,0.,1.));
#6751=DIRECTION('',(1.,0.,0.));
#6752=DIRECTION('center_axis',(1.,0.,0.));
#6753=DIRECTION('ref_axis',(0.,1.,0.));
#6754=DIRECTION('',(0.,1.,0.));
#6755=DIRECTION('',(0.,1.,0.));
#6756=DIRECTION('center_axis',(0.,0.,1.));
#6757=DIRECTION('ref_axis',(1.,0.,0.));
#6758=DIRECTION('center_axis',(0.,0.,1.));
#6759=DIRECTION('ref_axis',(1.,0.,0.));
#6760=DIRECTION('',(0.,0.,-1.));
#6761=DIRECTION('center_axis',(0.,0.,1.));
#6762=DIRECTION('ref_axis',(1.,0.,0.));
#6763=DIRECTION('center_axis',(0.,0.,1.));
#6764=DIRECTION('ref_axis',(1.,0.,0.));
#6765=DIRECTION('center_axis',(0.,0.,-1.));
#6766=DIRECTION('ref_axis',(1.,0.,0.));
#6767=DIRECTION('center_axis',(0.,0.,1.));
#6768=DIRECTION('ref_axis',(1.,0.,0.));
#6769=DIRECTION('center_axis',(0.,0.,-1.));
#6770=DIRECTION('ref_axis',(1.,0.,0.));
#6771=DIRECTION('',(0.,0.,-1.));
#6772=DIRECTION('center_axis',(0.,0.,1.));
#6773=DIRECTION('ref_axis',(-1.,1.22464679914735E-16,0.));
#6774=DIRECTION('center_axis',(0.,0.,1.));
#6775=DIRECTION('ref_axis',(1.,0.,0.));
#6776=DIRECTION('center_axis',(0.,0.,1.));
#6777=DIRECTION('ref_axis',(1.,0.,0.));
#6778=DIRECTION('center_axis',(0.,0.,1.));
#6779=DIRECTION('ref_axis',(1.,0.,0.));
#6780=DIRECTION('center_axis',(0.,0.,1.));
#6781=DIRECTION('ref_axis',(1.,0.,0.));
#6782=DIRECTION('axis',(0.,0.,1.));
#6783=DIRECTION('refdir',(1.,0.,0.));
#6784=DIRECTION('center_axis',(0.,0.,1.));
#6785=DIRECTION('ref_axis',(1.,0.,0.));
#6786=DIRECTION('center_axis',(0.,0.,1.));
#6787=DIRECTION('ref_axis',(1.,0.,0.));
#6788=DIRECTION('',(0.,0.,-1.));
#6789=DIRECTION('center_axis',(0.,0.,-1.));
#6790=DIRECTION('ref_axis',(1.,0.,0.));
#6791=DIRECTION('center_axis',(0.,0.,1.));
#6792=DIRECTION('ref_axis',(1.,0.,0.));
#6793=DIRECTION('center_axis',(0.,0.,1.));
#6794=DIRECTION('ref_axis',(1.,0.,0.));
#6795=DIRECTION('center_axis',(0.,0.,1.));
#6796=DIRECTION('ref_axis',(1.,0.,0.));
#6797=DIRECTION('',(0.,0.,-1.));
#6798=DIRECTION('center_axis',(0.,0.,1.));
#6799=DIRECTION('ref_axis',(1.,0.,0.));
#6800=DIRECTION('center_axis',(0.,0.,1.));
#6801=DIRECTION('ref_axis',(1.,0.,0.));
#6802=DIRECTION('center_axis',(0.,0.,1.));
#6803=DIRECTION('ref_axis',(1.,0.,0.));
#6804=DIRECTION('axis',(0.,0.,1.));
#6805=DIRECTION('refdir',(1.,0.,0.));
#6806=DIRECTION('center_axis',(0.,0.,1.));
#6807=DIRECTION('ref_axis',(1.,0.,0.));
#6808=DIRECTION('center_axis',(0.,0.,1.));
#6809=DIRECTION('ref_axis',(1.,0.,0.));
#6810=DIRECTION('',(0.,0.,-1.));
#6811=DIRECTION('center_axis',(0.,0.,1.));
#6812=DIRECTION('ref_axis',(1.,0.,0.));
#6813=DIRECTION('center_axis',(0.,0.,1.));
#6814=DIRECTION('ref_axis',(1.,0.,0.));
#6815=DIRECTION('center_axis',(0.,0.,1.));
#6816=DIRECTION('ref_axis',(1.,0.,0.));
#6817=DIRECTION('axis',(0.,0.,1.));
#6818=DIRECTION('refdir',(1.,0.,0.));
#6819=DIRECTION('axis',(0.,0.,1.));
#6820=DIRECTION('refdir',(1.,0.,0.));
#6821=DIRECTION('center_axis',(0.,-1.,0.));
#6822=DIRECTION('ref_axis',(0.,0.,-1.));
#6823=DIRECTION('center_axis',(0.,-1.,0.));
#6824=DIRECTION('ref_axis',(1.,0.,0.));
#6825=DIRECTION('center_axis',(0.,-1.,0.));
#6826=DIRECTION('ref_axis',(1.,0.,0.));
#6827=DIRECTION('center_axis',(1.,0.,1.22464679914735E-16));
#6828=DIRECTION('ref_axis',(-1.22464679914735E-16,0.,1.));
#6829=DIRECTION('center_axis',(0.,1.,0.));
#6830=DIRECTION('ref_axis',(1.,0.,0.));
#6831=DIRECTION('center_axis',(0.,1.,0.));
#6832=DIRECTION('ref_axis',(1.,0.,0.));
#6833=DIRECTION('center_axis',(0.,-1.,0.));
#6834=DIRECTION('ref_axis',(1.,0.,0.));
#6835=DIRECTION('',(0.,1.,0.));
#6836=DIRECTION('center_axis',(0.,-1.,0.));
#6837=DIRECTION('ref_axis',(1.,0.,0.));
#6838=DIRECTION('center_axis',(0.,-1.,0.));
#6839=DIRECTION('ref_axis',(1.,0.,0.));
#6840=DIRECTION('center_axis',(0.,-1.,0.));
#6841=DIRECTION('ref_axis',(1.,0.,0.));
#6842=DIRECTION('',(0.,1.,0.));
#6843=DIRECTION('center_axis',(0.,-1.,0.));
#6844=DIRECTION('ref_axis',(1.,0.,0.));
#6845=DIRECTION('center_axis',(0.,1.,0.));
#6846=DIRECTION('ref_axis',(1.,0.,0.));
#6847=DIRECTION('',(-0.707106781186547,0.707106781186548,-8.65956056235493E-17));
#6848=DIRECTION('center_axis',(0.,-1.,0.));
#6849=DIRECTION('ref_axis',(1.,0.,0.));
#6850=DIRECTION('center_axis',(0.,1.,0.));
#6851=DIRECTION('ref_axis',(0.,0.,1.));
#6852=DIRECTION('center_axis',(0.,-1.,0.));
#6853=DIRECTION('ref_axis',(1.,0.,0.));
#6854=DIRECTION('center_axis',(0.,-1.,0.));
#6855=DIRECTION('ref_axis',(1.,0.,0.));
#6856=DIRECTION('',(0.,1.,0.));
#6857=DIRECTION('center_axis',(0.,-1.,0.));
#6858=DIRECTION('ref_axis',(0.,0.,-1.));
#6859=DIRECTION('center_axis',(0.,-1.,0.));
#6860=DIRECTION('ref_axis',(1.,0.,0.));
#6861=DIRECTION('center_axis',(0.,-1.,0.));
#6862=DIRECTION('ref_axis',(1.,0.,0.));
#6863=DIRECTION('',(0.707106781186547,0.707106781186548,8.65956056235493E-17));
#6864=DIRECTION('axis',(0.,0.,1.));
#6865=DIRECTION('refdir',(1.,0.,0.));
#6866=DIRECTION('center_axis',(0.,-1.,0.));
#6867=DIRECTION('ref_axis',(0.,0.,-1.));
#6868=DIRECTION('center_axis',(0.,-1.,0.));
#6869=DIRECTION('ref_axis',(1.,0.,0.));
#6870=DIRECTION('center_axis',(0.,-1.,0.));
#6871=DIRECTION('ref_axis',(1.,0.,0.));
#6872=DIRECTION('center_axis',(1.,0.,1.22464679914735E-16));
#6873=DIRECTION('ref_axis',(-1.22464679914735E-16,0.,1.));
#6874=DIRECTION('center_axis',(0.,1.,0.));
#6875=DIRECTION('ref_axis',(1.,0.,0.));
#6876=DIRECTION('center_axis',(0.,1.,0.));
#6877=DIRECTION('ref_axis',(1.,0.,0.));
#6878=DIRECTION('center_axis',(0.,-1.,0.));
#6879=DIRECTION('ref_axis',(1.,0.,0.));
#6880=DIRECTION('center_axis',(0.,-1.,0.));
#6881=DIRECTION('ref_axis',(1.,0.,0.));
#6882=DIRECTION('',(0.,1.,0.));
#6883=DIRECTION('center_axis',(0.,1.,0.));
#6884=DIRECTION('ref_axis',(0.,0.,1.));
#6885=DIRECTION('center_axis',(0.,-1.,0.));
#6886=DIRECTION('ref_axis',(1.,0.,0.));
#6887=DIRECTION('center_axis',(0.,-1.,0.));
#6888=DIRECTION('ref_axis',(1.,0.,0.));
#6889=DIRECTION('center_axis',(0.,-1.,0.));
#6890=DIRECTION('ref_axis',(1.,0.,0.));
#6891=DIRECTION('center_axis',(0.,-1.,0.));
#6892=DIRECTION('ref_axis',(1.,0.,0.));
#6893=DIRECTION('',(0.707106781186548,0.707106781186547,8.65956056235494E-17));
#6894=DIRECTION('center_axis',(0.,-1.,0.));
#6895=DIRECTION('ref_axis',(1.,0.,0.));
#6896=DIRECTION('center_axis',(0.,-1.,0.));
#6897=DIRECTION('ref_axis',(1.,0.,0.));
#6898=DIRECTION('',(0.,1.,0.));
#6899=DIRECTION('center_axis',(0.,1.,0.));
#6900=DIRECTION('ref_axis',(1.,0.,0.));
#6901=DIRECTION('center_axis',(0.,-1.,0.));
#6902=DIRECTION('ref_axis',(1.,0.,0.));
#6903=DIRECTION('',(-0.707106781186548,0.707106781186547,-8.65956056235494E-17));
#6904=DIRECTION('center_axis',(0.,-1.,0.));
#6905=DIRECTION('ref_axis',(0.,0.,-1.));
#6906=DIRECTION('center_axis',(0.,-1.,0.));
#6907=DIRECTION('ref_axis',(1.,0.,0.));
#6908=DIRECTION('',(0.,1.,0.));
#6909=DIRECTION('axis',(0.,0.,1.));
#6910=DIRECTION('refdir',(1.,0.,0.));
#6911=DIRECTION('center_axis',(0.,0.,1.));
#6912=DIRECTION('ref_axis',(1.,0.,0.));
#6913=DIRECTION('center_axis',(1.22464679914735E-16,-1.,0.));
#6914=DIRECTION('ref_axis',(-1.,-1.22464679914735E-16,0.));
#6915=DIRECTION('center_axis',(0.707106781186548,0.,0.707106781186548));
#6916=DIRECTION('ref_axis',(0.707106781186548,0.,-0.707106781186548));
#6917=DIRECTION('center_axis',(8.65956056235494E-17,-1.,-8.65956056235493E-17));
#6918=DIRECTION('ref_axis',(-0.707106781186547,-1.22464679914735E-16,0.707106781186547));
#6919=DIRECTION('center_axis',(1.,0.,0.));
#6920=DIRECTION('ref_axis',(6.12323399573676E-17,0.,-1.));
#6921=DIRECTION('center_axis',(7.49879891330929E-33,-1.,-1.22464679914735E-16));
#6922=DIRECTION('ref_axis',(-6.12323399573676E-17,-1.22464679914735E-16,
1.));
#6923=DIRECTION('center_axis',(0.707106781186548,0.,-0.707106781186548));
#6924=DIRECTION('ref_axis',(-0.707106781186548,0.,-0.707106781186548));
#6925=DIRECTION('center_axis',(-8.65956056235493E-17,-1.,-8.65956056235494E-17));
#6926=DIRECTION('ref_axis',(0.707106781186547,-1.22464679914735E-16,0.707106781186547));
#6927=DIRECTION('center_axis',(0.,0.,-1.));
#6928=DIRECTION('ref_axis',(-1.,0.,-1.22464679914735E-16));
#6929=DIRECTION('center_axis',(-1.22464679914735E-16,-1.,-1.49975978266186E-32));
#6930=DIRECTION('ref_axis',(1.,-1.22464679914735E-16,1.22464679914735E-16));
#6931=DIRECTION('center_axis',(-0.707106781186547,0.,-0.707106781186548));
#6932=DIRECTION('ref_axis',(-0.707106781186548,0.,0.707106781186547));
#6933=DIRECTION('center_axis',(-8.65956056235493E-17,-1.,8.65956056235493E-17));
#6934=DIRECTION('ref_axis',(0.707106781186548,-1.22464679914735E-16,-0.707106781186547));
#6935=DIRECTION('center_axis',(-1.,0.,0.));
#6936=DIRECTION('ref_axis',(-1.83697019872103E-16,0.,1.));
#6937=DIRECTION('center_axis',(-2.24963967399279E-32,-1.,1.22464679914735E-16));
#6938=DIRECTION('ref_axis',(1.83697019872103E-16,-1.22464679914735E-16,
-1.));
#6939=DIRECTION('center_axis',(-0.707106781186548,0.,0.707106781186548));
#6940=DIRECTION('ref_axis',(0.707106781186547,0.,0.707106781186548));
#6941=DIRECTION('center_axis',(8.65956056235493E-17,-1.,8.65956056235493E-17));
#6942=DIRECTION('ref_axis',(-0.707106781186547,-1.22464679914735E-16,-0.707106781186548));
#6943=DIRECTION('axis',(0.,0.,1.));
#6944=DIRECTION('refdir',(1.,0.,0.));
#6945=DIRECTION('center_axis',(0.,0.,1.));
#6946=DIRECTION('ref_axis',(1.,0.,0.));
#6947=DIRECTION('center_axis',(0.,-1.,0.));
#6948=DIRECTION('ref_axis',(0.,0.,-1.));
#6949=DIRECTION('center_axis',(0.,-1.,0.));
#6950=DIRECTION('ref_axis',(0.,0.,-1.));
#6951=DIRECTION('center_axis',(0.,1.,0.));
#6952=DIRECTION('ref_axis',(1.,0.,0.));
#6953=DIRECTION('center_axis',(0.,1.,0.));
#6954=DIRECTION('ref_axis',(1.,0.,0.));
#6955=DIRECTION('center_axis',(0.,1.,0.));
#6956=DIRECTION('ref_axis',(1.,0.,0.));
#6957=DIRECTION('center_axis',(0.,1.,0.));
#6958=DIRECTION('ref_axis',(1.,0.,0.));
#6959=DIRECTION('',(0.,-1.,0.));
#6960=DIRECTION('center_axis',(0.,-1.,0.));
#6961=DIRECTION('ref_axis',(1.,0.,0.));
#6962=DIRECTION('center_axis',(0.,1.,0.));
#6963=DIRECTION('ref_axis',(1.,0.,0.));
#6964=DIRECTION('center_axis',(0.,1.,0.));
#6965=DIRECTION('ref_axis',(1.,0.,0.));
#6966=DIRECTION('center_axis',(0.,1.,0.));
#6967=DIRECTION('ref_axis',(1.,0.,0.));
#6968=DIRECTION('center_axis',(0.,1.,0.));
#6969=DIRECTION('ref_axis',(1.,0.,0.));
#6970=DIRECTION('center_axis',(0.,1.,0.));
#6971=DIRECTION('ref_axis',(1.,0.,0.));
#6972=DIRECTION('center_axis',(0.,1.,0.));
#6973=DIRECTION('ref_axis',(1.,0.,0.));
#6974=DIRECTION('center_axis',(0.,-1.,0.));
#6975=DIRECTION('ref_axis',(1.,0.,0.));
#6976=DIRECTION('center_axis',(0.,-1.,0.));
#6977=DIRECTION('ref_axis',(0.,0.,-1.));
#6978=DIRECTION('center_axis',(6.12323399573677E-17,0.,1.));
#6979=DIRECTION('ref_axis',(1.,0.,0.));
#6980=DIRECTION('center_axis',(0.,-1.,0.));
#6981=DIRECTION('ref_axis',(0.,0.,-1.));
#6982=DIRECTION('center_axis',(0.,1.,0.));
#6983=DIRECTION('ref_axis',(1.,0.,0.));
#6984=DIRECTION('center_axis',(0.,-1.,0.));
#6985=DIRECTION('ref_axis',(1.,0.,0.));
#6986=DIRECTION('center_axis',(0.,-1.,0.));
#6987=DIRECTION('ref_axis',(0.,0.,-1.));
#6988=DIRECTION('center_axis',(0.,0.,1.));
#6989=DIRECTION('ref_axis',(1.,0.,0.));
#6990=DIRECTION('center_axis',(0.,-1.,0.));
#6991=DIRECTION('ref_axis',(0.,0.,-1.));
#6992=DIRECTION('center_axis',(0.,1.,0.));
#6993=DIRECTION('ref_axis',(1.,0.,0.));
#6994=DIRECTION('center_axis',(0.,-1.,0.));
#6995=DIRECTION('ref_axis',(1.,0.,0.));
#6996=DIRECTION('center_axis',(0.,-1.,0.));
#6997=DIRECTION('ref_axis',(0.,0.,-1.));
#6998=DIRECTION('center_axis',(0.,0.,1.));
#6999=DIRECTION('ref_axis',(1.,0.,0.));
#7000=DIRECTION('center_axis',(0.,-1.,0.));
#7001=DIRECTION('ref_axis',(0.,0.,-1.));
#7002=DIRECTION('center_axis',(0.,1.,0.));
#7003=DIRECTION('ref_axis',(1.,0.,0.));
#7004=DIRECTION('center_axis',(0.,-1.,0.));
#7005=DIRECTION('ref_axis',(1.,0.,0.));
#7006=DIRECTION('center_axis',(0.,-1.,0.));
#7007=DIRECTION('ref_axis',(0.,0.,-1.));
#7008=DIRECTION('center_axis',(0.,0.,1.));
#7009=DIRECTION('ref_axis',(1.,0.,0.));
#7010=DIRECTION('center_axis',(0.,-1.,0.));
#7011=DIRECTION('ref_axis',(0.,0.,-1.));
#7012=DIRECTION('center_axis',(0.,1.,0.));
#7013=DIRECTION('ref_axis',(1.,0.,0.));
#7014=DIRECTION('center_axis',(0.,-1.,0.));
#7015=DIRECTION('ref_axis',(1.,0.,0.));
#7016=DIRECTION('center_axis',(0.,-1.,0.));
#7017=DIRECTION('ref_axis',(0.,0.,-1.));
#7018=DIRECTION('center_axis',(6.12323399573676E-17,0.,1.));
#7019=DIRECTION('ref_axis',(1.,0.,0.));
#7020=DIRECTION('center_axis',(0.,-1.,0.));
#7021=DIRECTION('ref_axis',(0.,0.,-1.));
#7022=DIRECTION('center_axis',(0.,1.,0.));
#7023=DIRECTION('ref_axis',(1.,0.,0.));
#7024=DIRECTION('center_axis',(0.,-1.,0.));
#7025=DIRECTION('ref_axis',(1.,0.,0.));
#7026=DIRECTION('center_axis',(0.,-1.,0.));
#7027=DIRECTION('ref_axis',(0.,0.,-1.));
#7028=DIRECTION('center_axis',(0.,0.,1.));
#7029=DIRECTION('ref_axis',(1.,0.,0.));
#7030=DIRECTION('center_axis',(0.,-1.,0.));
#7031=DIRECTION('ref_axis',(0.,0.,-1.));
#7032=DIRECTION('center_axis',(0.,1.,0.));
#7033=DIRECTION('ref_axis',(1.,0.,0.));
#7034=DIRECTION('center_axis',(0.,1.,0.));
#7035=DIRECTION('ref_axis',(1.,0.,0.));
#7036=DIRECTION('',(0.,1.,0.));
#7037=DIRECTION('center_axis',(0.,-1.,0.));
#7038=DIRECTION('ref_axis',(1.,0.,0.));
#7039=DIRECTION('center_axis',(0.,-1.,0.));
#7040=DIRECTION('ref_axis',(1.,0.,0.));
#7041=DIRECTION('center_axis',(0.,1.,0.));
#7042=DIRECTION('ref_axis',(1.,0.,0.));
#7043=DIRECTION('center_axis',(0.,-1.,0.));
#7044=DIRECTION('ref_axis',(0.,0.,-1.));
#7045=DIRECTION('center_axis',(0.,0.,1.));
#7046=DIRECTION('ref_axis',(1.,0.,0.));
#7047=DIRECTION('center_axis',(0.,-1.,0.));
#7048=DIRECTION('ref_axis',(0.,0.,-1.));
#7049=DIRECTION('center_axis',(0.,-1.,0.));
#7050=DIRECTION('ref_axis',(-1.,0.,0.));
#7051=DIRECTION('center_axis',(0.,1.,0.));
#7052=DIRECTION('ref_axis',(1.,0.,0.));
#7053=DIRECTION('axis',(0.,0.,1.));
#7054=DIRECTION('refdir',(1.,0.,0.));
#7055=DIRECTION('center_axis',(0.,1.,0.));
#7056=DIRECTION('ref_axis',(0.,0.,1.));
#7057=DIRECTION('center_axis',(0.,-1.,0.));
#7058=DIRECTION('ref_axis',(1.,0.,0.));
#7059=DIRECTION('center_axis',(0.,-1.,0.));
#7060=DIRECTION('ref_axis',(1.,0.,0.));
#7061=DIRECTION('center_axis',(0.,-1.,0.));
#7062=DIRECTION('ref_axis',(1.,0.,0.));
#7063=DIRECTION('center_axis',(0.,-1.,0.));
#7064=DIRECTION('ref_axis',(1.,0.,0.));
#7065=DIRECTION('',(0.,1.,0.));
#7066=DIRECTION('center_axis',(0.,-1.,0.));
#7067=DIRECTION('ref_axis',(0.,0.,-1.));
#7068=DIRECTION('center_axis',(0.,-1.,0.));
#7069=DIRECTION('ref_axis',(1.,0.,0.));
#7070=DIRECTION('center_axis',(0.,-1.,0.));
#7071=DIRECTION('ref_axis',(1.,0.,0.));
#7072=DIRECTION('',(0.,1.,0.));
#7073=DIRECTION('center_axis',(0.,1.,0.));
#7074=DIRECTION('ref_axis',(0.,0.,1.));
#7075=DIRECTION('center_axis',(0.,-1.,0.));
#7076=DIRECTION('ref_axis',(1.,0.,0.));
#7077=DIRECTION('center_axis',(0.,-1.,0.));
#7078=DIRECTION('ref_axis',(1.,0.,0.));
#7079=DIRECTION('center_axis',(0.,-1.,0.));
#7080=DIRECTION('ref_axis',(1.,0.,0.));
#7081=DIRECTION('center_axis',(0.,-1.,0.));
#7082=DIRECTION('ref_axis',(1.,0.,0.));
#7083=DIRECTION('',(0.,1.,0.));
#7084=DIRECTION('center_axis',(0.,-1.,0.));
#7085=DIRECTION('ref_axis',(0.,0.,-1.));
#7086=DIRECTION('center_axis',(0.,-1.,0.));
#7087=DIRECTION('ref_axis',(1.,0.,0.));
#7088=DIRECTION('center_axis',(0.,-1.,0.));
#7089=DIRECTION('ref_axis',(1.,0.,0.));
#7090=DIRECTION('',(0.,1.,0.));
#7091=DIRECTION('',(0.,0.,1.));
#7092=DIRECTION('',(1.,0.,0.));
#7093=DIRECTION('',(0.,0.,1.));
#7094=DIRECTION('',(1.,0.,0.));
#7095=DIRECTION('',(0.,0.,1.));
#7096=DIRECTION('',(1.,0.,0.));
#7097=DIRECTION('',(0.,0.,1.));
#7098=DIRECTION('',(1.,0.,0.));
#7099=DIRECTION('',(0.,0.,1.));
#7100=DIRECTION('',(1.,0.,0.));
#7101=DIRECTION('axis',(0.,0.,1.));
#7102=DIRECTION('refdir',(1.,0.,0.));
#7103=DIRECTION('axis',(0.,0.,1.));
#7104=DIRECTION('refdir',(1.,0.,0.));
#7105=DIRECTION('center_axis',(0.,1.,0.));
#7106=DIRECTION('ref_axis',(1.,0.,0.));
#7107=DIRECTION('center_axis',(0.,1.,0.));
#7108=DIRECTION('ref_axis',(1.,0.,0.));
#7109=DIRECTION('',(0.,1.,0.));
#7110=DIRECTION('center_axis',(0.,-1.,0.));
#7111=DIRECTION('ref_axis',(1.,0.,0.));
#7112=DIRECTION('center_axis',(0.,1.,0.));
#7113=DIRECTION('ref_axis',(1.,0.,0.));
#7114=DIRECTION('center_axis',(0.,1.,0.));
#7115=DIRECTION('ref_axis',(1.,0.,0.));
#7116=DIRECTION('center_axis',(0.,1.,0.));
#7117=DIRECTION('ref_axis',(1.,0.,0.));
#7118=DIRECTION('',(0.,1.,0.));
#7119=DIRECTION('center_axis',(0.,1.,0.));
#7120=DIRECTION('ref_axis',(1.,0.,0.));
#7121=DIRECTION('center_axis',(0.,1.,0.));
#7122=DIRECTION('ref_axis',(1.,0.,0.));
#7123=DIRECTION('center_axis',(0.,1.,0.));
#7124=DIRECTION('ref_axis',(1.,0.,0.));
#7125=DIRECTION('center_axis',(0.,1.,0.));
#7126=DIRECTION('ref_axis',(1.,0.,0.));
#7127=DIRECTION('center_axis',(0.,1.,0.));
#7128=DIRECTION('ref_axis',(1.,0.,0.));
#7129=DIRECTION('center_axis',(0.,1.,0.));
#7130=DIRECTION('ref_axis',(1.,0.,0.));
#7131=DIRECTION('',(0.,-1.,0.));
#7132=DIRECTION('center_axis',(0.,-1.,0.));
#7133=DIRECTION('ref_axis',(1.,0.,0.));
#7134=DIRECTION('center_axis',(0.,1.,0.));
#7135=DIRECTION('ref_axis',(1.,0.,0.));
#7136=DIRECTION('center_axis',(0.,1.,0.));
#7137=DIRECTION('ref_axis',(1.,0.,0.));
#7138=DIRECTION('center_axis',(0.,-1.,0.));
#7139=DIRECTION('ref_axis',(1.,0.,0.));
#7140=DIRECTION('center_axis',(0.,1.,0.));
#7141=DIRECTION('ref_axis',(1.,0.,0.));
#7142=DIRECTION('center_axis',(0.,1.,0.));
#7143=DIRECTION('ref_axis',(1.,0.,0.));
#7144=DIRECTION('',(0.,-1.,0.));
#7145=DIRECTION('center_axis',(0.,1.,0.));
#7146=DIRECTION('ref_axis',(1.,0.,0.));
#7147=DIRECTION('',(0.,-1.,0.));
#7148=DIRECTION('center_axis',(0.,1.,0.));
#7149=DIRECTION('ref_axis',(1.,0.,0.));
#7150=DIRECTION('center_axis',(0.,1.,0.));
#7151=DIRECTION('ref_axis',(1.,0.,0.));
#7152=DIRECTION('center_axis',(0.,1.,0.));
#7153=DIRECTION('ref_axis',(1.,0.,0.));
#7154=DIRECTION('',(0.,-1.,0.));
#7155=DIRECTION('center_axis',(0.,1.,0.));
#7156=DIRECTION('ref_axis',(1.,0.,0.));
#7157=DIRECTION('center_axis',(0.,1.,0.));
#7158=DIRECTION('ref_axis',(1.,0.,0.));
#7159=DIRECTION('center_axis',(0.,1.,0.));
#7160=DIRECTION('ref_axis',(1.,0.,0.));
#7161=DIRECTION('center_axis',(0.,1.,0.));
#7162=DIRECTION('ref_axis',(1.,0.,0.));
#7163=DIRECTION('',(0.,-1.,0.));
#7164=DIRECTION('center_axis',(0.,1.,0.));
#7165=DIRECTION('ref_axis',(1.,0.,0.));
#7166=DIRECTION('center_axis',(0.,1.,0.));
#7167=DIRECTION('ref_axis',(1.,0.,0.));
#7168=DIRECTION('center_axis',(0.,1.,0.));
#7169=DIRECTION('ref_axis',(1.,0.,0.));
#7170=DIRECTION('axis',(0.,0.,1.));
#7171=DIRECTION('refdir',(1.,0.,0.));
#7172=DIRECTION('center_axis',(0.,1.,0.));
#7173=DIRECTION('ref_axis',(1.,0.,0.));
#7174=DIRECTION('center_axis',(0.,1.,0.));
#7175=DIRECTION('ref_axis',(1.,0.,0.));
#7176=DIRECTION('',(0.,1.,0.));
#7177=DIRECTION('center_axis',(0.,-1.,0.));
#7178=DIRECTION('ref_axis',(1.,0.,0.));
#7179=DIRECTION('center_axis',(0.,1.,0.));
#7180=DIRECTION('ref_axis',(1.,0.,0.));
#7181=DIRECTION('',(0.,-1.,0.));
#7182=DIRECTION('center_axis',(0.,1.,0.));
#7183=DIRECTION('ref_axis',(1.,0.,0.));
#7184=DIRECTION('',(0.,1.,0.));
#7185=DIRECTION('center_axis',(0.,1.,0.));
#7186=DIRECTION('ref_axis',(1.,0.,0.));
#7187=DIRECTION('center_axis',(0.,1.,0.));
#7188=DIRECTION('ref_axis',(1.,0.,0.));
#7189=DIRECTION('',(-1.,0.,0.));
#7190=DIRECTION('center_axis',(0.,1.,0.));
#7191=DIRECTION('ref_axis',(1.,0.,0.));
#7192=DIRECTION('center_axis',(0.,1.,0.));
#7193=DIRECTION('ref_axis',(1.,0.,0.));
#7194=DIRECTION('',(1.,0.,0.));
#7195=DIRECTION('center_axis',(0.,-1.,0.));
#7196=DIRECTION('ref_axis',(1.,0.,0.));
#7197=DIRECTION('center_axis',(0.,0.,1.));
#7198=DIRECTION('ref_axis',(1.,0.,0.));
#7199=DIRECTION('',(1.,0.,0.));
#7200=DIRECTION('',(0.,1.,0.));
#7201=DIRECTION('center_axis',(0.,0.,-1.));
#7202=DIRECTION('ref_axis',(-1.,0.,0.));
#7203=DIRECTION('',(0.,-1.,0.));
#7204=DIRECTION('',(-1.,0.,0.));
#7205=DIRECTION('center_axis',(0.,1.,0.));
#7206=DIRECTION('ref_axis',(0.,0.,1.));
#7207=DIRECTION('center_axis',(0.,1.,0.));
#7208=DIRECTION('ref_axis',(1.,0.,0.));
#7209=DIRECTION('center_axis',(0.,1.,0.));
#7210=DIRECTION('ref_axis',(1.,0.,0.));
#7211=DIRECTION('center_axis',(0.,-1.,0.));
#7212=DIRECTION('ref_axis',(1.,0.,0.));
#7213=DIRECTION('',(0.,-1.,0.));
#7214=DIRECTION('center_axis',(0.,1.,0.));
#7215=DIRECTION('ref_axis',(1.,0.,0.));
#7216=DIRECTION('center_axis',(0.,1.,0.));
#7217=DIRECTION('ref_axis',(1.,0.,0.));
#7218=DIRECTION('',(0.,-1.,0.));
#7219=DIRECTION('center_axis',(0.,1.,0.));
#7220=DIRECTION('ref_axis',(1.,0.,0.));
#7221=DIRECTION('axis',(0.,0.,1.));
#7222=DIRECTION('refdir',(1.,0.,0.));
#7223=DIRECTION('center_axis',(0.,1.,0.));
#7224=DIRECTION('ref_axis',(1.,0.,0.));
#7225=DIRECTION('center_axis',(0.,1.,0.));
#7226=DIRECTION('ref_axis',(1.,0.,0.));
#7227=DIRECTION('',(0.,1.,0.));
#7228=DIRECTION('center_axis',(0.,-1.,0.));
#7229=DIRECTION('ref_axis',(1.,0.,0.));
#7230=DIRECTION('center_axis',(0.,1.,0.));
#7231=DIRECTION('ref_axis',(1.,0.,0.));
#7232=DIRECTION('center_axis',(0.,1.,0.));
#7233=DIRECTION('ref_axis',(1.,0.,0.));
#7234=DIRECTION('center_axis',(0.,1.,0.));
#7235=DIRECTION('ref_axis',(1.,0.,0.));
#7236=DIRECTION('',(0.,-1.,0.));
#7237=DIRECTION('center_axis',(0.,1.,0.));
#7238=DIRECTION('ref_axis',(1.,0.,0.));
#7239=DIRECTION('center_axis',(0.,1.,0.));
#7240=DIRECTION('ref_axis',(1.,0.,0.));
#7241=DIRECTION('center_axis',(0.,1.,0.));
#7242=DIRECTION('ref_axis',(1.,0.,0.));
#7243=DIRECTION('axis',(0.,0.,1.));
#7244=DIRECTION('refdir',(1.,0.,0.));
#7245=DIRECTION('center_axis',(0.,1.,0.));
#7246=DIRECTION('ref_axis',(1.,0.,0.));
#7247=DIRECTION('center_axis',(0.,-1.,0.));
#7248=DIRECTION('ref_axis',(1.,0.,0.));
#7249=DIRECTION('',(0.,-1.,0.));
#7250=DIRECTION('center_axis',(0.,-1.,0.));
#7251=DIRECTION('ref_axis',(1.,0.,0.));
#7252=DIRECTION('center_axis',(0.,1.,0.));
#7253=DIRECTION('ref_axis',(1.,0.,0.));
#7254=DIRECTION('center_axis',(0.,1.,0.));
#7255=DIRECTION('ref_axis',(1.,0.,0.));
#7256=DIRECTION('',(0.,-1.,0.));
#7257=DIRECTION('center_axis',(0.,1.,0.));
#7258=DIRECTION('ref_axis',(1.,0.,0.));
#7259=DIRECTION('center_axis',(0.,1.,0.));
#7260=DIRECTION('ref_axis',(1.,0.,0.));
#7261=DIRECTION('center_axis',(0.,1.,0.));
#7262=DIRECTION('ref_axis',(1.,0.,0.));
#7263=DIRECTION('axis',(0.,0.,1.));
#7264=DIRECTION('refdir',(1.,0.,0.));
#7265=DIRECTION('center_axis',(0.,1.,0.));
#7266=DIRECTION('ref_axis',(1.,0.,0.));
#7267=DIRECTION('center_axis',(0.,-1.,0.));
#7268=DIRECTION('ref_axis',(1.,0.,0.));
#7269=DIRECTION('',(0.,-1.,0.));
#7270=DIRECTION('center_axis',(0.,-1.,0.));
#7271=DIRECTION('ref_axis',(1.,0.,0.));
#7272=DIRECTION('center_axis',(0.,1.,0.));
#7273=DIRECTION('ref_axis',(1.,0.,0.));
#7274=DIRECTION('center_axis',(0.,1.,0.));
#7275=DIRECTION('ref_axis',(1.,0.,0.));
#7276=DIRECTION('',(0.,-1.,0.));
#7277=DIRECTION('center_axis',(0.,1.,0.));
#7278=DIRECTION('ref_axis',(1.,0.,0.));
#7279=DIRECTION('center_axis',(0.,1.,0.));
#7280=DIRECTION('ref_axis',(1.,0.,0.));
#7281=DIRECTION('center_axis',(0.,1.,0.));
#7282=DIRECTION('ref_axis',(1.,0.,0.));
#7283=DIRECTION('axis',(0.,0.,1.));
#7284=DIRECTION('refdir',(1.,0.,0.));
#7285=DIRECTION('center_axis',(0.,1.,0.));
#7286=DIRECTION('ref_axis',(0.,0.,1.));
#7287=DIRECTION('center_axis',(0.,-1.,0.));
#7288=DIRECTION('ref_axis',(1.,0.,0.));
#7289=DIRECTION('center_axis',(0.,-1.,0.));
#7290=DIRECTION('ref_axis',(1.,0.,0.));
#7291=DIRECTION('center_axis',(0.,-1.,0.));
#7292=DIRECTION('ref_axis',(1.,0.,0.));
#7293=DIRECTION('',(0.707106781186547,0.707106781186548,8.65956056235493E-17));
#7294=DIRECTION('center_axis',(0.,-1.,0.));
#7295=DIRECTION('ref_axis',(1.,0.,0.));
#7296=DIRECTION('center_axis',(0.,-1.,0.));
#7297=DIRECTION('ref_axis',(1.,0.,0.));
#7298=DIRECTION('',(0.,1.,0.));
#7299=DIRECTION('center_axis',(0.,1.,0.));
#7300=DIRECTION('ref_axis',(1.,0.,0.));
#7301=DIRECTION('center_axis',(0.,-1.,0.));
#7302=DIRECTION('ref_axis',(1.,0.,0.));
#7303=DIRECTION('',(-0.707106781186547,0.707106781186548,-8.65956056235493E-17));
#7304=DIRECTION('center_axis',(0.,-1.,0.));
#7305=DIRECTION('ref_axis',(0.,0.,-1.));
#7306=DIRECTION('center_axis',(0.,-1.,0.));
#7307=DIRECTION('ref_axis',(1.,0.,0.));
#7308=DIRECTION('center_axis',(0.,1.,0.));
#7309=DIRECTION('ref_axis',(1.,0.,0.));
#7310=DIRECTION('center_axis',(0.,1.,0.));
#7311=DIRECTION('ref_axis',(1.,0.,0.));
#7312=DIRECTION('',(-0.447213595499958,0.894427190999916,-5.47678698264203E-17));
#7313=DIRECTION('center_axis',(0.,-1.,0.));
#7314=DIRECTION('ref_axis',(1.,0.,0.));
#7315=DIRECTION('center_axis',(0.,1.,0.));
#7316=DIRECTION('ref_axis',(1.,0.,0.));
#7317=DIRECTION('',(0.,1.,0.));
#7318=DIRECTION('center_axis',(0.,1.,0.));
#7319=DIRECTION('ref_axis',(1.,0.,0.));
#7320=DIRECTION('center_axis',(0.,-1.,0.));
#7321=DIRECTION('ref_axis',(1.,0.,0.));
#7322=DIRECTION('',(-0.707106781186547,0.707106781186548,-8.65956056235493E-17));
#7323=DIRECTION('center_axis',(0.,-1.,0.));
#7324=DIRECTION('ref_axis',(0.,0.,-1.));
#7325=DIRECTION('center_axis',(0.866025403784439,0.,-0.5));
#7326=DIRECTION('ref_axis',(0.5,0.,0.866025403784439));
#7327=DIRECTION('',(-0.5,0.,-0.866025403784439));
#7328=DIRECTION('',(0.,-1.,0.));
#7329=DIRECTION('',(0.5,0.,0.866025403784439));
#7330=DIRECTION('',(0.,-1.,0.));
#7331=DIRECTION('center_axis',(1.60246890531964E-16,0.,-1.));
#7332=DIRECTION('ref_axis',(1.,0.,1.60246890531964E-16));
#7333=DIRECTION('',(-1.,0.,-1.60246890531964E-16));
#7334=DIRECTION('',(0.,-1.,0.));
#7335=DIRECTION('',(1.,0.,1.60246890531964E-16));
#7336=DIRECTION('center_axis',(-0.866025403784439,0.,-0.5));
#7337=DIRECTION('ref_axis',(0.5,0.,-0.866025403784439));
#7338=DIRECTION('',(-0.5,0.,0.866025403784439));
#7339=DIRECTION('',(0.,-1.,0.));
#7340=DIRECTION('',(0.5,0.,-0.866025403784439));
#7341=DIRECTION('center_axis',(-0.866025403784439,0.,0.5));
#7342=DIRECTION('ref_axis',(-0.5,0.,-0.866025403784439));
#7343=DIRECTION('',(0.5,0.,0.866025403784439));
#7344=DIRECTION('',(0.,-1.,0.));
#7345=DIRECTION('',(-0.5,0.,-0.866025403784439));
#7346=DIRECTION('center_axis',(-1.60246890531964E-16,0.,1.));
#7347=DIRECTION('ref_axis',(-1.,0.,-1.60246890531964E-16));
#7348=DIRECTION('',(1.,0.,1.60246890531964E-16));
#7349=DIRECTION('',(0.,-1.,0.));
#7350=DIRECTION('',(-1.,0.,-1.60246890531964E-16));
#7351=DIRECTION('center_axis',(0.866025403784439,0.,0.5));
#7352=DIRECTION('ref_axis',(-0.5,0.,0.866025403784439));
#7353=DIRECTION('',(0.5,0.,-0.866025403784439));
#7354=DIRECTION('',(-0.5,0.,0.866025403784439));
#7355=DIRECTION('center_axis',(0.,1.,0.));
#7356=DIRECTION('ref_axis',(1.,0.,0.));
#7357=DIRECTION('center_axis',(0.,-1.,0.));
#7358=DIRECTION('ref_axis',(0.,0.,-1.));
#7359=DIRECTION('axis',(0.,0.,1.));
#7360=DIRECTION('refdir',(1.,0.,0.));
#7361=DIRECTION('center_axis',(0.866025403784439,0.,-0.5));
#7362=DIRECTION('ref_axis',(0.5,0.,0.866025403784439));
#7363=DIRECTION('',(-0.5,0.,-0.866025403784439));
#7364=DIRECTION('',(0.,-1.,0.));
#7365=DIRECTION('',(0.5,0.,0.866025403784439));
#7366=DIRECTION('',(0.,-1.,0.));
#7367=DIRECTION('center_axis',(1.60246890531964E-16,0.,-1.));
#7368=DIRECTION('ref_axis',(1.,0.,1.60246890531964E-16));
#7369=DIRECTION('',(-1.,0.,-1.60246890531964E-16));
#7370=DIRECTION('',(0.,-1.,0.));
#7371=DIRECTION('',(1.,0.,1.60246890531964E-16));
#7372=DIRECTION('center_axis',(-0.866025403784439,0.,-0.5));
#7373=DIRECTION('ref_axis',(0.5,0.,-0.866025403784439));
#7374=DIRECTION('',(-0.5,0.,0.866025403784439));
#7375=DIRECTION('',(0.,-1.,0.));
#7376=DIRECTION('',(0.5,0.,-0.866025403784439));
#7377=DIRECTION('center_axis',(-0.866025403784439,0.,0.5));
#7378=DIRECTION('ref_axis',(-0.5,0.,-0.866025403784439));
#7379=DIRECTION('',(0.5,0.,0.866025403784439));
#7380=DIRECTION('',(0.,-1.,0.));
#7381=DIRECTION('',(-0.5,0.,-0.866025403784439));
#7382=DIRECTION('center_axis',(-1.60246890531964E-16,0.,1.));
#7383=DIRECTION('ref_axis',(-1.,0.,-1.60246890531964E-16));
#7384=DIRECTION('',(1.,0.,1.60246890531964E-16));
#7385=DIRECTION('',(0.,-1.,0.));
#7386=DIRECTION('',(-1.,0.,-1.60246890531964E-16));
#7387=DIRECTION('center_axis',(0.866025403784439,0.,0.5));
#7388=DIRECTION('ref_axis',(-0.5,0.,0.866025403784439));
#7389=DIRECTION('',(0.5,0.,-0.866025403784439));
#7390=DIRECTION('',(-0.5,0.,0.866025403784439));
#7391=DIRECTION('center_axis',(0.,1.,0.));
#7392=DIRECTION('ref_axis',(1.,0.,0.));
#7393=DIRECTION('center_axis',(0.,-1.,0.));
#7394=DIRECTION('ref_axis',(0.,0.,-1.));
#7395=DIRECTION('center_axis',(0.,1.,0.));
#7396=DIRECTION('ref_axis',(1.,0.,0.));
#7397=DIRECTION('center_axis',(0.,1.,0.));
#7398=DIRECTION('ref_axis',(1.,0.,0.));
#7399=DIRECTION('center_axis',(0.,1.,0.));
#7400=DIRECTION('ref_axis',(0.,0.,1.));
#7401=DIRECTION('center_axis',(0.,-1.,0.));
#7402=DIRECTION('ref_axis',(1.,0.,0.));
#7403=DIRECTION('center_axis',(0.,-1.,0.));
#7404=DIRECTION('ref_axis',(1.,0.,0.));
#7405=DIRECTION('center_axis',(0.,-1.,0.));
#7406=DIRECTION('ref_axis',(1.,0.,0.));
#7407=DIRECTION('',(0.707106781186547,0.707106781186548,8.65956056235493E-17));
#7408=DIRECTION('center_axis',(0.,-1.,0.));
#7409=DIRECTION('ref_axis',(1.,0.,0.));
#7410=DIRECTION('center_axis',(0.,-1.,0.));
#7411=DIRECTION('ref_axis',(1.,0.,0.));
#7412=DIRECTION('',(0.,1.,0.));
#7413=DIRECTION('center_axis',(0.,1.,0.));
#7414=DIRECTION('ref_axis',(1.,0.,0.));
#7415=DIRECTION('center_axis',(0.,-1.,0.));
#7416=DIRECTION('ref_axis',(1.,0.,0.));
#7417=DIRECTION('',(-0.707106781186547,0.707106781186548,-8.65956056235493E-17));
#7418=DIRECTION('center_axis',(0.,-1.,0.));
#7419=DIRECTION('ref_axis',(0.,0.,-1.));
#7420=DIRECTION('center_axis',(0.,-1.,0.));
#7421=DIRECTION('ref_axis',(1.,0.,0.));
#7422=DIRECTION('center_axis',(0.,1.,0.));
#7423=DIRECTION('ref_axis',(1.,0.,0.));
#7424=DIRECTION('center_axis',(0.,1.,0.));
#7425=DIRECTION('ref_axis',(1.,0.,0.));
#7426=DIRECTION('',(-0.447213595499958,0.894427190999916,-5.47678698264203E-17));
#7427=DIRECTION('center_axis',(0.,-1.,0.));
#7428=DIRECTION('ref_axis',(1.,0.,0.));
#7429=DIRECTION('',(0.,1.,0.));
#7430=DIRECTION('',(0.,0.,1.));
#7431=DIRECTION('',(1.,0.,0.));
#7432=DIRECTION('',(0.,0.,1.));
#7433=DIRECTION('',(1.,0.,0.));
#7434=DIRECTION('',(0.,0.,1.));
#7435=DIRECTION('',(1.,0.,0.));
#7436=DIRECTION('',(0.,0.,1.));
#7437=DIRECTION('',(1.,0.,0.));
#7438=DIRECTION('',(0.,0.,1.));
#7439=DIRECTION('',(1.,0.,0.));
#7440=DIRECTION('',(0.,0.,1.));
#7441=DIRECTION('',(1.,0.,0.));
#7442=DIRECTION('',(0.,0.,1.));
#7443=DIRECTION('',(1.,0.,0.));
#7444=DIRECTION('',(0.,-1.,2.22044604925031E-16));
#7445=DIRECTION('',(1.,0.,0.));
#7446=DIRECTION('',(0.,-1.,2.22044604925031E-16));
#7447=DIRECTION('',(1.,0.,0.));
#7448=DIRECTION('',(0.,1.,2.22044604925031E-16));
#7449=DIRECTION('',(1.,0.,0.));
#7450=DIRECTION('',(0.,1.,2.22044604925031E-16));
#7451=DIRECTION('',(1.,0.,0.));
#7452=DIRECTION('',(0.,1.,2.22044604925031E-16));
#7453=DIRECTION('',(1.,0.,0.));
#7454=DIRECTION('',(0.,1.,2.22044604925031E-16));
#7455=DIRECTION('',(1.,0.,0.));
#7456=DIRECTION('',(0.,-1.,2.22044604925031E-16));
#7457=DIRECTION('',(1.,0.,0.));
#7458=DIRECTION('',(0.,-1.,2.22044604925031E-16));
#7459=DIRECTION('',(1.,0.,0.));
#7460=DIRECTION('',(0.,-1.,2.22044604925031E-16));
#7461=DIRECTION('',(1.,0.,0.));
#7462=DIRECTION('',(0.,-1.,2.22044604925031E-16));
#7463=DIRECTION('',(1.,0.,0.));
#7464=DIRECTION('',(0.,0.,1.));
#7465=DIRECTION('',(1.,0.,0.));
#7466=DIRECTION('',(0.,0.,1.));
#7467=DIRECTION('',(1.,0.,0.));
#7468=DIRECTION('',(0.,0.,1.));
#7469=DIRECTION('',(1.,0.,0.));
#7470=DIRECTION('',(0.,0.,1.));
#7471=DIRECTION('',(1.,0.,0.));
#7472=DIRECTION('',(0.,0.,1.));
#7473=DIRECTION('',(1.,0.,0.));
#7474=DIRECTION('',(0.,0.,1.));
#7475=DIRECTION('',(1.,0.,0.));
#7476=DIRECTION('',(0.,0.,1.));
#7477=DIRECTION('',(-1.,1.22464679914735E-16,0.));
#7478=DIRECTION('',(0.,0.,1.));
#7479=DIRECTION('',(1.,0.,0.));
#7480=DIRECTION('',(0.,0.,1.));
#7481=DIRECTION('',(1.,0.,0.));
#7482=DIRECTION('',(0.,0.,1.));
#7483=DIRECTION('',(1.,0.,0.));
#7484=DIRECTION('',(0.,0.,1.));
#7485=DIRECTION('',(1.,0.,0.));
#7486=CARTESIAN_POINT('',(0.,0.,0.));
#7487=CARTESIAN_POINT('',(0.,0.,0.));
#7488=CARTESIAN_POINT('',(0.,0.,0.));
#7489=CARTESIAN_POINT('Origin',(-0.989949493661167,-0.989949493661166,-0.1));
#7490=CARTESIAN_POINT('',(-1.19994949366117,-0.989949493661166,0.));
#7491=CARTESIAN_POINT('Origin',(-0.989949493661167,-0.989949493661166,0.));
#7492=CARTESIAN_POINT('',(-1.19994949366117,-0.989949493661166,1.));
#7493=CARTESIAN_POINT('',(-1.19994949366117,-0.989949493661166,-0.1));
#7494=CARTESIAN_POINT('Origin',(-0.989949493661167,-0.989949493661166,1.));
#7495=CARTESIAN_POINT('Origin',(-0.989949493661166,0.989949493661167,-0.1));
#7496=CARTESIAN_POINT('',(-1.19994949366117,0.989949493661167,0.));
#7497=CARTESIAN_POINT('Origin',(-0.989949493661166,0.989949493661167,0.));
#7498=CARTESIAN_POINT('',(-1.19994949366117,0.989949493661167,1.));
#7499=CARTESIAN_POINT('',(-1.19994949366117,0.989949493661167,-0.1));
#7500=CARTESIAN_POINT('Origin',(-0.989949493661166,0.989949493661167,1.));
#7501=CARTESIAN_POINT('Origin',(0.989949493661167,0.989949493661166,-0.1));
#7502=CARTESIAN_POINT('',(0.779949493661167,0.989949493661166,0.));
#7503=CARTESIAN_POINT('Origin',(0.989949493661167,0.989949493661166,0.));
#7504=CARTESIAN_POINT('',(0.779949493661167,0.989949493661166,1.));
#7505=CARTESIAN_POINT('',(0.779949493661167,0.989949493661166,-0.1));
#7506=CARTESIAN_POINT('Origin',(0.989949493661167,0.989949493661166,1.));
#7507=CARTESIAN_POINT('Origin',(0.989949493661166,-0.989949493661167,-0.1));
#7508=CARTESIAN_POINT('',(0.779949493661166,-0.989949493661167,0.));
#7509=CARTESIAN_POINT('Origin',(0.989949493661166,-0.989949493661167,0.));
#7510=CARTESIAN_POINT('',(0.779949493661166,-0.989949493661167,1.));
#7511=CARTESIAN_POINT('',(0.779949493661166,-0.989949493661167,-0.1));
#7512=CARTESIAN_POINT('Origin',(0.989949493661166,-0.989949493661167,1.));
#7513=CARTESIAN_POINT('Origin',(16.,15.5,0.));
#7514=CARTESIAN_POINT('',(16.,15.5,0.));
#7515=CARTESIAN_POINT('',(-4.5,15.5,0.));
#7516=CARTESIAN_POINT('',(16.,15.5,0.));
#7517=CARTESIAN_POINT('',(-4.5,15.5,1.));
#7518=CARTESIAN_POINT('',(-4.5,15.5,0.));
#7519=CARTESIAN_POINT('',(16.,15.5,1.));
#7520=CARTESIAN_POINT('',(16.,15.5,1.));
#7521=CARTESIAN_POINT('',(16.,15.5,0.));
#7522=CARTESIAN_POINT('Origin',(16.,-5.5,0.));
#7523=CARTESIAN_POINT('',(16.,-5.5,0.));
#7524=CARTESIAN_POINT('',(16.,-5.5,0.));
#7525=CARTESIAN_POINT('',(16.,-5.5,1.));
#7526=CARTESIAN_POINT('',(16.,-5.5,1.));
#7527=CARTESIAN_POINT('',(16.,-5.5,0.));
#7528=CARTESIAN_POINT('Origin',(-4.5,-5.5,0.));
#7529=CARTESIAN_POINT('',(-4.5,-5.5,0.));
#7530=CARTESIAN_POINT('',(-4.5,-5.5,0.));
#7531=CARTESIAN_POINT('',(-4.5,-5.5,1.));
#7532=CARTESIAN_POINT('',(-4.5,-5.5,1.));
#7533=CARTESIAN_POINT('',(-4.5,-5.5,0.));
#7534=CARTESIAN_POINT('Origin',(-4.5,15.5,0.));
#7535=CARTESIAN_POINT('',(-4.5,15.5,0.));
#7536=CARTESIAN_POINT('',(-4.5,15.5,1.));
#7537=CARTESIAN_POINT('Origin',(5.75,5.,1.));
#7538=CARTESIAN_POINT('Origin',(5.75,5.,0.));
#7539=CARTESIAN_POINT('',(0.,0.,0.));
#7540=CARTESIAN_POINT('Origin',(-3.5,15.5,-0.8));
#7541=CARTESIAN_POINT('',(-3.5,15.5,-0.8));
#7542=CARTESIAN_POINT('',(-4.5,15.5,-0.8));
#7543=CARTESIAN_POINT('',(-3.5,15.5,-0.8));
#7544=CARTESIAN_POINT('',(-4.5,15.5,0.));
#7545=CARTESIAN_POINT('',(-4.5,15.5,-0.8));
#7546=CARTESIAN_POINT('',(-3.5,15.5,0.));
#7547=CARTESIAN_POINT('',(-3.5,15.5,0.));
#7548=CARTESIAN_POINT('',(-3.5,15.5,-0.8));
#7549=CARTESIAN_POINT('Origin',(-3.5,-5.5,-0.8));
#7550=CARTESIAN_POINT('',(-3.5,-5.5,-0.8));
#7551=CARTESIAN_POINT('',(-3.5,-5.5,-0.8));
#7552=CARTESIAN_POINT('',(-3.5,-5.5,0.));
#7553=CARTESIAN_POINT('',(-3.5,-5.5,0.));
#7554=CARTESIAN_POINT('',(-3.5,-5.5,-0.8));
#7555=CARTESIAN_POINT('Origin',(-4.5,-5.5,-0.8));
#7556=CARTESIAN_POINT('',(-4.5,-5.5,-0.8));
#7557=CARTESIAN_POINT('',(-4.5,-5.5,-0.8));
#7558=CARTESIAN_POINT('',(-4.5,-5.5,0.));
#7559=CARTESIAN_POINT('',(-4.5,-5.5,0.));
#7560=CARTESIAN_POINT('',(-4.5,-5.5,-0.8));
#7561=CARTESIAN_POINT('Origin',(-4.5,15.5,-0.8));
#7562=CARTESIAN_POINT('',(-4.5,15.5,-0.8));
#7563=CARTESIAN_POINT('',(-4.5,15.5,0.));
#7564=CARTESIAN_POINT('Origin',(-4.,5.,0.));
#7565=CARTESIAN_POINT('Origin',(-4.,5.,-0.8));
#7566=CARTESIAN_POINT('',(0.,0.,0.));
#7567=CARTESIAN_POINT('Origin',(16.,15.5,-0.8));
#7568=CARTESIAN_POINT('',(16.,15.5,-0.8));
#7569=CARTESIAN_POINT('',(15.,15.5,-0.8));
#7570=CARTESIAN_POINT('',(16.,15.5,-0.8));
#7571=CARTESIAN_POINT('',(15.,15.5,0.));
#7572=CARTESIAN_POINT('',(15.,15.5,-0.8));
#7573=CARTESIAN_POINT('',(16.,15.5,0.));
#7574=CARTESIAN_POINT('',(16.,15.5,0.));
#7575=CARTESIAN_POINT('',(16.,15.5,-0.8));
#7576=CARTESIAN_POINT('Origin',(16.,-5.5,-0.8));
#7577=CARTESIAN_POINT('',(16.,-5.5,-0.8));
#7578=CARTESIAN_POINT('',(16.,-5.5,-0.8));
#7579=CARTESIAN_POINT('',(16.,-5.5,0.));
#7580=CARTESIAN_POINT('',(16.,-5.5,0.));
#7581=CARTESIAN_POINT('',(16.,-5.5,-0.8));
#7582=CARTESIAN_POINT('Origin',(15.,-5.5,-0.8));
#7583=CARTESIAN_POINT('',(15.,-5.5,-0.8));
#7584=CARTESIAN_POINT('',(15.,-5.5,-0.8));
#7585=CARTESIAN_POINT('',(15.,-5.5,0.));
#7586=CARTESIAN_POINT('',(15.,-5.5,0.));
#7587=CARTESIAN_POINT('',(15.,-5.5,-0.8));
#7588=CARTESIAN_POINT('Origin',(15.,15.5,-0.8));
#7589=CARTESIAN_POINT('',(15.,15.5,-0.8));
#7590=CARTESIAN_POINT('',(15.,15.5,0.));
#7591=CARTESIAN_POINT('Origin',(15.5,5.,0.));
#7592=CARTESIAN_POINT('Origin',(15.5,5.,-0.8));
#7593=CARTESIAN_POINT('',(0.,0.,0.));
#7594=CARTESIAN_POINT('Origin',(-0.989949493661167,-0.989949493661166,1.5));
#7595=CARTESIAN_POINT('',(-1.01060488132664,-1.48952266644008,1.5));
#7596=CARTESIAN_POINT('',(-1.48952266644008,-1.01060488132664,1.5));
#7597=CARTESIAN_POINT('Origin',(0.,0.,1.5));
#7598=CARTESIAN_POINT('Origin',(-0.989949493661167,-0.989949493661166,1.5));
#7599=CARTESIAN_POINT('',(-1.26494949366117,-0.989949493661166,1.5));
#7600=CARTESIAN_POINT('Origin',(-0.989949493661167,-0.989949493661166,1.5));
#7601=CARTESIAN_POINT('Origin',(-0.989949493661167,-0.989949493661166,1.5));
#7602=CARTESIAN_POINT('',(-1.01060488132664,-1.48952266644008,2.));
#7603=CARTESIAN_POINT('',(-1.01060488132664,-1.48952266644008,1.5));
#7604=CARTESIAN_POINT('',(-1.48952266644008,-1.01060488132664,2.));
#7605=CARTESIAN_POINT('Origin',(-0.989949493661167,-0.989949493661166,2.));
#7606=CARTESIAN_POINT('',(-1.48952266644008,-1.01060488132664,1.5));
#7607=CARTESIAN_POINT('Origin',(-0.989949493661166,0.989949493661167,1.5));
#7608=CARTESIAN_POINT('',(-1.48952266644008,1.01060488132664,1.5));
#7609=CARTESIAN_POINT('',(-1.01060488132664,1.48952266644008,1.5));
#7610=CARTESIAN_POINT('Origin',(0.,0.,1.5));
#7611=CARTESIAN_POINT('Origin',(-0.989949493661166,0.989949493661167,1.5));
#7612=CARTESIAN_POINT('',(-1.26494949366117,0.989949493661167,1.5));
#7613=CARTESIAN_POINT('Origin',(-0.989949493661166,0.989949493661167,1.5));
#7614=CARTESIAN_POINT('Origin',(-0.989949493661166,0.989949493661167,1.5));
#7615=CARTESIAN_POINT('',(-1.48952266644008,1.01060488132664,2.));
#7616=CARTESIAN_POINT('',(-1.48952266644008,1.01060488132664,1.5));
#7617=CARTESIAN_POINT('',(-1.01060488132664,1.48952266644008,2.));
#7618=CARTESIAN_POINT('Origin',(-0.989949493661166,0.989949493661167,2.));
#7619=CARTESIAN_POINT('',(-1.01060488132664,1.48952266644008,1.5));
#7620=CARTESIAN_POINT('Origin',(0.989949493661167,0.989949493661166,1.5));
#7621=CARTESIAN_POINT('',(1.01060488132664,1.48952266644008,1.5));
#7622=CARTESIAN_POINT('',(1.48952266644008,1.01060488132664,1.5));
#7623=CARTESIAN_POINT('Origin',(0.,0.,1.5));
#7624=CARTESIAN_POINT('Origin',(0.989949493661167,0.989949493661166,1.5));
#7625=CARTESIAN_POINT('',(0.714949493661166,0.989949493661166,1.5));
#7626=CARTESIAN_POINT('Origin',(0.989949493661167,0.989949493661166,1.5));
#7627=CARTESIAN_POINT('Origin',(0.989949493661167,0.989949493661166,1.5));
#7628=CARTESIAN_POINT('',(1.01060488132664,1.48952266644008,2.));
#7629=CARTESIAN_POINT('',(1.01060488132664,1.48952266644008,1.5));
#7630=CARTESIAN_POINT('',(1.48952266644008,1.01060488132664,2.));
#7631=CARTESIAN_POINT('Origin',(0.989949493661167,0.989949493661166,2.));
#7632=CARTESIAN_POINT('',(1.48952266644008,1.01060488132664,1.5));
#7633=CARTESIAN_POINT('Origin',(0.989949493661166,-0.989949493661167,1.5));
#7634=CARTESIAN_POINT('',(1.48952266644008,-1.01060488132664,1.5));
#7635=CARTESIAN_POINT('',(1.01060488132664,-1.48952266644008,1.5));
#7636=CARTESIAN_POINT('Origin',(0.,0.,1.5));
#7637=CARTESIAN_POINT('Origin',(0.989949493661166,-0.989949493661167,1.5));
#7638=CARTESIAN_POINT('',(0.714949493661166,-0.989949493661167,1.5));
#7639=CARTESIAN_POINT('Origin',(0.989949493661166,-0.989949493661167,1.5));
#7640=CARTESIAN_POINT('Origin',(0.989949493661166,-0.989949493661167,1.5));
#7641=CARTESIAN_POINT('',(1.48952266644008,-1.01060488132664,2.));
#7642=CARTESIAN_POINT('',(1.48952266644008,-1.01060488132664,1.5));
#7643=CARTESIAN_POINT('',(1.01060488132664,-1.48952266644008,2.));
#7644=CARTESIAN_POINT('Origin',(0.989949493661166,-0.989949493661167,2.));
#7645=CARTESIAN_POINT('',(1.01060488132664,-1.48952266644008,1.5));
#7646=CARTESIAN_POINT('Origin',(0.,0.,2.));
#7647=CARTESIAN_POINT('Origin',(0.,0.,2.));
#7648=CARTESIAN_POINT('Origin',(0.,0.,2.));
#7649=CARTESIAN_POINT('Origin',(0.,0.,2.));
#7650=CARTESIAN_POINT('',(-1.8,-2.20436423846524E-16,2.));
#7651=CARTESIAN_POINT('Origin',(0.,0.,2.));
#7652=CARTESIAN_POINT('Origin',(0.,0.,2.));
#7653=CARTESIAN_POINT('',(-0.5,-6.12323399573677E-17,2.));
#7654=CARTESIAN_POINT('Origin',(0.,0.,2.));
#7655=CARTESIAN_POINT('Origin',(0.,0.,1.));
#7656=CARTESIAN_POINT('',(-1.8,-2.20436423846524E-16,1.));
#7657=CARTESIAN_POINT('',(-1.8,-2.20436423846524E-16,1.));
#7658=CARTESIAN_POINT('Origin',(0.,0.,1.));
#7659=CARTESIAN_POINT('Origin',(-2.31008116418808,-5.,9.02921777339027));
#7660=CARTESIAN_POINT('',(-2.61008116418808,-1.4,9.02921777339027));
#7661=CARTESIAN_POINT('Origin',(-2.31008116418808,-1.4,9.02921777339027));
#7662=CARTESIAN_POINT('',(-2.61008116418808,-5.,9.02921777339027));
#7663=CARTESIAN_POINT('',(-2.61008116418808,-5.,9.02921777339027));
#7664=CARTESIAN_POINT('Origin',(-2.31008116418808,-5.,9.02921777339027));
#7665=CARTESIAN_POINT('Origin',(-2.31008116418808,-1.4,9.02921777339027));
#7666=CARTESIAN_POINT('Origin',(-1.5,-5.,13.5));
#7667=CARTESIAN_POINT('',(-1.,-5.,18.5));
#7668=CARTESIAN_POINT('',(-1.,-5.,19.));
#7669=CARTESIAN_POINT('',(-1.,-5.,16.));
#7670=CARTESIAN_POINT('',(0.,-5.,18.5));
#7671=CARTESIAN_POINT('',(-0.75,-5.,18.5));
#7672=CARTESIAN_POINT('',(0.,-5.,8.));
#7673=CARTESIAN_POINT('',(0.,-5.,8.));
#7674=CARTESIAN_POINT('',(-3.,-5.,8.));
#7675=CARTESIAN_POINT('',(-3.,-5.,8.));
#7676=CARTESIAN_POINT('',(-3.,-5.,19.));
#7677=CARTESIAN_POINT('',(-3.,-5.,19.));
#7678=CARTESIAN_POINT('',(0.,-5.,19.));
#7679=CARTESIAN_POINT('Origin',(0.,-5.5,19.));
#7680=CARTESIAN_POINT('',(0.,-5.5,18.5));
#7681=CARTESIAN_POINT('',(0.,-4.125,18.5));
#7682=CARTESIAN_POINT('',(0.,-5.5,8.));
#7683=CARTESIAN_POINT('',(0.,-5.5,8.));
#7684=CARTESIAN_POINT('',(0.,-5.5,8.));
#7685=CARTESIAN_POINT('Origin',(-3.,-5.5,8.));
#7686=CARTESIAN_POINT('',(-3.,-5.5,19.));
#7687=CARTESIAN_POINT('',(-3.,-5.5,8.));
#7688=CARTESIAN_POINT('',(-3.,-5.5,19.));
#7689=CARTESIAN_POINT('',(-3.,-5.5,19.));
#7690=CARTESIAN_POINT('',(-3.,-5.5,8.));
#7691=CARTESIAN_POINT('Origin',(0.,-5.5,8.));
#7692=CARTESIAN_POINT('',(-3.,-5.5,8.));
#7693=CARTESIAN_POINT('Origin',(-1.,0.,18.5));
#7694=CARTESIAN_POINT('',(-1.,0.,19.));
#7695=CARTESIAN_POINT('',(-1.,0.,19.));
#7696=CARTESIAN_POINT('',(-1.,0.,18.5));
#7697=CARTESIAN_POINT('',(-1.,0.,18.5));
#7698=CARTESIAN_POINT('',(-1.,0.,18.5));
#7699=CARTESIAN_POINT('Origin',(0.,0.,19.));
#7700=CARTESIAN_POINT('',(1.,-5.5,19.));
#7701=CARTESIAN_POINT('',(0.,-5.5,19.));
#7702=CARTESIAN_POINT('',(1.,0.,19.));
#7703=CARTESIAN_POINT('',(1.,-5.5,19.));
#7704=CARTESIAN_POINT('',(0.5,0.,19.));
#7705=CARTESIAN_POINT('',(1.,0.,19.));
#7706=CARTESIAN_POINT('',(-0.5,-6.12323399573677E-17,19.));
#7707=CARTESIAN_POINT('Origin',(0.,0.,19.));
#7708=CARTESIAN_POINT('',(1.,0.,19.));
#7709=CARTESIAN_POINT('Origin',(1.,0.,18.5));
#7710=CARTESIAN_POINT('',(-0.5,0.,18.5));
#7711=CARTESIAN_POINT('',(-0.5,0.,12.));
#7712=CARTESIAN_POINT('',(1.,0.,18.5));
#7713=CARTESIAN_POINT('Origin',(1.,0.,18.5));
#7714=CARTESIAN_POINT('',(0.5,0.,18.5));
#7715=CARTESIAN_POINT('',(0.5,0.,12.));
#7716=CARTESIAN_POINT('',(1.,0.,18.5));
#7717=CARTESIAN_POINT('',(1.,0.,18.5));
#7718=CARTESIAN_POINT('',(1.,0.,18.5));
#7719=CARTESIAN_POINT('Origin',(1.,-5.5,18.5));
#7720=CARTESIAN_POINT('',(1.,-5.5,18.5));
#7721=CARTESIAN_POINT('',(1.,-5.5,18.5));
#7722=CARTESIAN_POINT('',(1.,-5.5,18.5));
#7723=CARTESIAN_POINT('Origin',(-1.,-5.5,18.5));
#7724=CARTESIAN_POINT('',(-1.,-5.5,18.5));
#7725=CARTESIAN_POINT('Origin',(0.,-2.75,18.5));
#7726=CARTESIAN_POINT('Origin',(0.,0.,18.5));
#7727=CARTESIAN_POINT('Origin',(0.,0.,12.));
#7728=CARTESIAN_POINT('',(-0.5,-6.12323399573677E-17,12.));
#7729=CARTESIAN_POINT('',(-0.5,-6.12323399573677E-17,12.));
#7730=CARTESIAN_POINT('Origin',(0.,0.,12.));
#7731=CARTESIAN_POINT('',(0.,-0.5,12.2));
#7732=CARTESIAN_POINT('',(0.,-0.5,12.7));
#7733=CARTESIAN_POINT('',(0.,-0.5,12.));
#7734=CARTESIAN_POINT('',(0.3,-0.4,12.7));
#7735=CARTESIAN_POINT('Origin',(0.,0.,12.7));
#7736=CARTESIAN_POINT('',(0.3,-0.4,12.2));
#7737=CARTESIAN_POINT('',(0.3,-0.4,12.));
#7738=CARTESIAN_POINT('Origin',(0.,0.,12.2));
#7739=CARTESIAN_POINT('',(0.,0.5,12.7));
#7740=CARTESIAN_POINT('',(0.,0.5,12.2));
#7741=CARTESIAN_POINT('',(0.,0.5,12.));
#7742=CARTESIAN_POINT('',(0.3,0.4,12.2));
#7743=CARTESIAN_POINT('Origin',(0.,0.,12.2));
#7744=CARTESIAN_POINT('',(0.3,0.4,12.7));
#7745=CARTESIAN_POINT('',(0.3,0.4,12.));
#7746=CARTESIAN_POINT('Origin',(0.,0.,12.7));
#7747=CARTESIAN_POINT('Origin',(2.,0.6,10.5));
#7748=CARTESIAN_POINT('',(1.695,0.7,10.5));
#7749=CARTESIAN_POINT('Origin',(2.,0.7,10.5));
#7750=CARTESIAN_POINT('',(1.695,1.4,10.5));
#7751=CARTESIAN_POINT('',(1.695,0.6,10.5));
#7752=CARTESIAN_POINT('Origin',(2.,1.4,10.5));
#7753=CARTESIAN_POINT('Origin',(1.,0.7,12.5));
#7754=CARTESIAN_POINT('',(3.,0.7,12.5));
#7755=CARTESIAN_POINT('',(3.,1.4,12.5));
#7756=CARTESIAN_POINT('',(3.,0.55,12.5));
#7757=CARTESIAN_POINT('',(3.5,0.7,12.5));
#7758=CARTESIAN_POINT('',(3.5,0.7,12.5));
#7759=CARTESIAN_POINT('',(3.5,1.4,12.5));
#7760=CARTESIAN_POINT('',(3.5,0.7,12.5));
#7761=CARTESIAN_POINT('',(3.5,1.4,12.5));
#7762=CARTESIAN_POINT('Origin',(1.,0.7,9.5));
#7763=CARTESIAN_POINT('',(1.,1.4,12.2));
#7764=CARTESIAN_POINT('',(1.,0.7,12.2));
#7765=CARTESIAN_POINT('',(1.,0.55,12.2));
#7766=CARTESIAN_POINT('',(1.,1.4,9.5));
#7767=CARTESIAN_POINT('',(1.,1.4,12.5));
#7768=CARTESIAN_POINT('',(1.,0.7,9.5));
#7769=CARTESIAN_POINT('',(1.,0.7,9.5));
#7770=CARTESIAN_POINT('',(1.,0.7,12.5));
#7771=CARTESIAN_POINT('Origin',(3.5,0.7,9.5));
#7772=CARTESIAN_POINT('',(3.5,0.7,9.5));
#7773=CARTESIAN_POINT('',(1.,0.7,9.5));
#7774=CARTESIAN_POINT('',(3.5,1.4,9.5));
#7775=CARTESIAN_POINT('',(1.,1.4,9.5));
#7776=CARTESIAN_POINT('',(3.5,0.7,9.5));
#7777=CARTESIAN_POINT('Origin',(3.5,0.7,12.5));
#7778=CARTESIAN_POINT('',(3.5,0.7,9.5));
#7779=CARTESIAN_POINT('',(3.5,1.4,9.5));
#7780=CARTESIAN_POINT('Origin',(2.25,0.7,11.));
#7781=CARTESIAN_POINT('',(3.,0.7,12.2));
#7782=CARTESIAN_POINT('',(2.625,0.7,12.2));
#7783=CARTESIAN_POINT('',(3.,0.7,11.85));
#7784=CARTESIAN_POINT('Origin',(3.,0.4,12.2));
#7785=CARTESIAN_POINT('',(3.,0.4,12.2));
#7786=CARTESIAN_POINT('',(3.,0.4,12.2));
#7787=CARTESIAN_POINT('',(0.,0.4,12.2));
#7788=CARTESIAN_POINT('',(0.,1.4,12.2));
#7789=CARTESIAN_POINT('',(0.,0.4,12.2));
#7790=CARTESIAN_POINT('',(0.,1.4,12.2));
#7791=CARTESIAN_POINT('Origin',(3.,0.4,12.7));
#7792=CARTESIAN_POINT('',(3.,1.4,12.7));
#7793=CARTESIAN_POINT('',(3.,1.4,12.2));
#7794=CARTESIAN_POINT('',(3.,0.4,12.7));
#7795=CARTESIAN_POINT('',(3.,0.4,12.7));
#7796=CARTESIAN_POINT('',(3.,0.4,12.2));
#7797=CARTESIAN_POINT('Origin',(0.,0.4,12.2));
#7798=CARTESIAN_POINT('',(0.,1.4,12.7));
#7799=CARTESIAN_POINT('',(0.,0.4,12.7));
#7800=CARTESIAN_POINT('',(0.,1.4,12.7));
#7801=CARTESIAN_POINT('Origin',(0.,0.4,12.7));
#7802=CARTESIAN_POINT('',(3.,0.4,12.7));
#7803=CARTESIAN_POINT('',(3.,1.4,12.7));
#7804=CARTESIAN_POINT('Origin',(1.5,1.4,12.45));
#7805=CARTESIAN_POINT('Origin',(1.5,0.4,12.45));
#7806=CARTESIAN_POINT('Origin',(2.,-1.5,10.5));
#7807=CARTESIAN_POINT('',(1.695,-1.4,10.5));
#7808=CARTESIAN_POINT('Origin',(2.,-1.4,10.5));
#7809=CARTESIAN_POINT('',(1.695,-0.7,10.5));
#7810=CARTESIAN_POINT('',(1.695,-1.5,10.5));
#7811=CARTESIAN_POINT('Origin',(2.,-0.7,10.5));
#7812=CARTESIAN_POINT('Origin',(2.25,-0.7,11.));
#7813=CARTESIAN_POINT('',(3.,-0.7,12.2));
#7814=CARTESIAN_POINT('',(1.,-0.7,12.2));
#7815=CARTESIAN_POINT('',(2.625,-0.7,12.2));
#7816=CARTESIAN_POINT('',(3.,-0.7,12.5));
#7817=CARTESIAN_POINT('',(3.,-0.7,11.85));
#7818=CARTESIAN_POINT('',(3.5,-0.7,12.5));
#7819=CARTESIAN_POINT('',(3.5,-0.7,12.5));
#7820=CARTESIAN_POINT('',(3.5,-0.7,9.5));
#7821=CARTESIAN_POINT('',(3.5,-0.7,9.5));
#7822=CARTESIAN_POINT('',(1.,-0.7,9.5));
#7823=CARTESIAN_POINT('',(1.,-0.7,9.5));
#7824=CARTESIAN_POINT('',(1.,-0.7,12.5));
#7825=CARTESIAN_POINT('Origin',(1.,-1.4,12.5));
#7826=CARTESIAN_POINT('',(3.,-1.4,12.5));
#7827=CARTESIAN_POINT('',(3.,-1.4,12.5));
#7828=CARTESIAN_POINT('',(3.5,-1.4,12.5));
#7829=CARTESIAN_POINT('',(3.5,-1.4,12.5));
#7830=CARTESIAN_POINT('',(3.5,-1.4,12.5));
#7831=CARTESIAN_POINT('Origin',(1.,-1.4,9.5));
#7832=CARTESIAN_POINT('',(1.,-1.4,12.2));
#7833=CARTESIAN_POINT('',(1.,-1.4,12.2));
#7834=CARTESIAN_POINT('',(1.,-1.4,9.5));
#7835=CARTESIAN_POINT('',(1.,-1.4,9.5));
#7836=CARTESIAN_POINT('',(1.,-1.4,12.5));
#7837=CARTESIAN_POINT('Origin',(3.5,-1.4,9.5));
#7838=CARTESIAN_POINT('',(3.5,-1.4,9.5));
#7839=CARTESIAN_POINT('',(1.,-1.4,9.5));
#7840=CARTESIAN_POINT('',(3.5,-1.4,9.5));
#7841=CARTESIAN_POINT('Origin',(3.5,-1.4,12.5));
#7842=CARTESIAN_POINT('',(3.5,-1.4,9.5));
#7843=CARTESIAN_POINT('Origin',(1.5,-1.4,12.45));
#7844=CARTESIAN_POINT('',(3.,-1.4,12.7));
#7845=CARTESIAN_POINT('',(3.,-1.4,12.2));
#7846=CARTESIAN_POINT('',(0.,-1.4,12.7));
#7847=CARTESIAN_POINT('',(3.,-1.4,12.7));
#7848=CARTESIAN_POINT('',(0.,-1.4,12.2));
#7849=CARTESIAN_POINT('',(0.,-1.4,12.7));
#7850=CARTESIAN_POINT('',(0.,-1.4,12.2));
#7851=CARTESIAN_POINT('Origin',(0.,-1.4,12.7));
#7852=CARTESIAN_POINT('',(0.,-1.4,12.7));
#7853=CARTESIAN_POINT('',(3.,-0.4,12.7));
#7854=CARTESIAN_POINT('',(3.,-1.4,12.7));
#7855=CARTESIAN_POINT('',(3.,-0.4,12.7));
#7856=CARTESIAN_POINT('Origin',(0.,-1.4,12.2));
#7857=CARTESIAN_POINT('',(0.,-1.4,12.2));
#7858=CARTESIAN_POINT('Origin',(3.,-1.4,12.2));
#7859=CARTESIAN_POINT('',(3.,-0.4,12.2));
#7860=CARTESIAN_POINT('',(0.,-0.4,12.2));
#7861=CARTESIAN_POINT('',(3.,-1.4,12.2));
#7862=CARTESIAN_POINT('Origin',(3.,-1.4,12.7));
#7863=CARTESIAN_POINT('',(3.,-0.4,12.2));
#7864=CARTESIAN_POINT('Origin',(1.5,-0.4,12.45));
#7865=CARTESIAN_POINT('Origin',(-0.989949493661167,-0.989949493661166,0.9));
#7866=CARTESIAN_POINT('',(-1.26494949366117,-0.989949493661166,1.));
#7867=CARTESIAN_POINT('Origin',(-0.989949493661167,-0.989949493661166,1.));
#7868=CARTESIAN_POINT('',(-1.26494949366117,-0.989949493661166,0.9));
#7869=CARTESIAN_POINT('Origin',(-0.989949493661166,0.989949493661167,0.9));
#7870=CARTESIAN_POINT('',(-1.26494949366117,0.989949493661167,1.));
#7871=CARTESIAN_POINT('Origin',(-0.989949493661166,0.989949493661167,1.));
#7872=CARTESIAN_POINT('',(-1.26494949366117,0.989949493661167,0.9));
#7873=CARTESIAN_POINT('Origin',(0.989949493661167,0.989949493661166,0.9));
#7874=CARTESIAN_POINT('',(0.714949493661166,0.989949493661166,1.));
#7875=CARTESIAN_POINT('Origin',(0.989949493661167,0.989949493661166,1.));
#7876=CARTESIAN_POINT('',(0.714949493661166,0.989949493661166,0.9));
#7877=CARTESIAN_POINT('Origin',(0.989949493661166,-0.989949493661167,0.9));
#7878=CARTESIAN_POINT('',(0.714949493661166,-0.989949493661167,1.));
#7879=CARTESIAN_POINT('Origin',(0.989949493661166,-0.989949493661167,1.));
#7880=CARTESIAN_POINT('',(0.714949493661166,-0.989949493661167,0.9));
#7881=CARTESIAN_POINT('Origin',(0.,0.,11.));
#7882=CARTESIAN_POINT('',(-0.7,-8.57252759403147E-17,11.));
#7883=CARTESIAN_POINT('Origin',(0.,0.,11.));
#7884=CARTESIAN_POINT('',(-0.5,-6.12323399573677E-17,11.));
#7885=CARTESIAN_POINT('Origin',(0.,0.,11.));
#7886=CARTESIAN_POINT('Origin',(0.,0.,11.));
#7887=CARTESIAN_POINT('',(-0.7,-8.57252759403147E-17,12.));
#7888=CARTESIAN_POINT('Origin',(0.,0.,12.));
#7889=CARTESIAN_POINT('',(-0.7,-8.57252759403147E-17,11.));
#7890=CARTESIAN_POINT('Origin',(0.,0.,12.));
#7891=CARTESIAN_POINT('Origin',(0.,0.,2.));
#7892=CARTESIAN_POINT('',(-0.5,-6.12323399573677E-17,2.));
#7893=CARTESIAN_POINT('Origin',(0.,0.,1.));
#7894=CARTESIAN_POINT('',(0.,0.,0.));
#7895=CARTESIAN_POINT('Origin',(14.,1.5,1.));
#7896=CARTESIAN_POINT('',(14.,1.5,1.));
#7897=CARTESIAN_POINT('',(10.,1.5,1.));
#7898=CARTESIAN_POINT('',(14.,1.5,1.));
#7899=CARTESIAN_POINT('',(10.,1.5,5.60303845));
#7900=CARTESIAN_POINT('',(10.,1.5,1.));
#7901=CARTESIAN_POINT('',(14.,1.5,5.60303845));
#7902=CARTESIAN_POINT('',(14.,1.5,5.60303845));
#7903=CARTESIAN_POINT('',(14.,1.5,1.));
#7904=CARTESIAN_POINT('Origin',(14.,-1.5,1.));
#7905=CARTESIAN_POINT('',(14.,-1.5,1.));
#7906=CARTESIAN_POINT('',(14.,-1.5,1.));
#7907=CARTESIAN_POINT('',(14.,-1.5,5.60303845));
#7908=CARTESIAN_POINT('',(14.,-1.5,5.60303845));
#7909=CARTESIAN_POINT('',(14.,-1.5,1.));
#7910=CARTESIAN_POINT('Origin',(10.,-1.5,1.));
#7911=CARTESIAN_POINT('',(10.,-1.5,1.));
#7912=CARTESIAN_POINT('',(10.,-1.5,1.));
#7913=CARTESIAN_POINT('',(10.,-1.5,5.60303845));
#7914=CARTESIAN_POINT('',(10.,-1.5,5.60303845));
#7915=CARTESIAN_POINT('',(10.,-1.5,1.));
#7916=CARTESIAN_POINT('Origin',(10.,1.5,1.));
#7917=CARTESIAN_POINT('',(10.,1.5,1.));
#7918=CARTESIAN_POINT('',(10.,1.5,5.60303845));
#7919=CARTESIAN_POINT('Origin',(12.,0.,5.60303845));
#7920=CARTESIAN_POINT('Origin',(12.,0.,1.));
#7921=CARTESIAN_POINT('',(0.,0.,0.));
#7922=CARTESIAN_POINT('Ctrl Pts',(0.999999464043874,0.00398121802342207,
2.00010574185718));
#7923=CARTESIAN_POINT('Ctrl Pts',(0.999974206061282,0.19160391813607,2.01007936209659));
#7924=CARTESIAN_POINT('Ctrl Pts',(0.892358674149497,0.565284907029969,2.03003975780563));
#7925=CARTESIAN_POINT('Ctrl Pts',(0.455908354460267,0.955754980387012,2.06005123671475));
#7926=CARTESIAN_POINT('Ctrl Pts',(-0.122563158588718,1.05404138225222,2.09012808179557));
#7927=CARTESIAN_POINT('Ctrl Pts',(-0.665982422429721,0.829161410069987,
2.12027227517451));
#7928=CARTESIAN_POINT('Ctrl Pts',(-1.00720268117277,0.348508238874394,2.15048257508427));
#7929=CARTESIAN_POINT('Ctrl Pts',(-1.04050120808252,-0.241264621011279,
2.18075912672908));
#7930=CARTESIAN_POINT('Ctrl Pts',(-0.754298406118339,-0.759496345182109,
2.21110138862918));
#7931=CARTESIAN_POINT('Ctrl Pts',(-0.235139085598783,-1.04662471701868,
2.24150905560043));
#7932=CARTESIAN_POINT('Ctrl Pts',(0.358466657407177,-1.0134893307861,2.27198163744466));
#7933=CARTESIAN_POINT('Ctrl Pts',(0.844481314225998,-0.668830870873697,
2.30251864881201));
#7934=CARTESIAN_POINT('Ctrl Pts',(1.07309171546203,-0.117397710656463,2.33311952120739));
#7935=CARTESIAN_POINT('Ctrl Pts',(0.973085863935879,0.472631726678538,2.36378364003101));
#7936=CARTESIAN_POINT('Ctrl Pts',(0.640186615940372,0.844850208282888,2.38938921676183));
#7937=CARTESIAN_POINT('Ctrl Pts',(0.285207254948024,1.00321211946817,2.40990460122644));
#7938=CARTESIAN_POINT('Ctrl Pts',(-0.00357278466147455,1.04413748919053,
2.42530650345941));
#7939=CARTESIAN_POINT('Ctrl Pts',(-0.292753333069628,1.00327492007872,2.4407236705559));
#7940=CARTESIAN_POINT('Ctrl Pts',(-0.559610149845377,0.883939984413932,
2.45615599894115));
#7941=CARTESIAN_POINT('Ctrl Pts',(-0.783072629292576,0.695150535469123,
2.47160338259101));
#7942=CARTESIAN_POINT('Ctrl Pts',(-0.9883155178948,0.388599518613216,2.49107446360262));
#7943=CARTESIAN_POINT('Ctrl Pts',(-1.06097928852007,0.0299698265249316,
2.50999804459158));
#7944=CARTESIAN_POINT('Ctrl Pts',(-1.00026874085688,-0.31207309433285,2.52837129391011));
#7945=CARTESIAN_POINT('Ctrl Pts',(-0.85772117693898,-0.628943233787528,
2.54675983289627));
#7946=CARTESIAN_POINT('Ctrl Pts',(-0.539023756454129,-0.940248430945502,
2.56977396086322));
#7947=CARTESIAN_POINT('Ctrl Pts',(-0.0813539710712336,-1.06875629404709,
2.59436218564022));
#7948=CARTESIAN_POINT('Ctrl Pts',(0.440709506996878,-0.995074461032676,
2.6220606386953));
#7949=CARTESIAN_POINT('Ctrl Pts',(0.881652173543376,-0.668351901468915,
2.64980261114177));
#7950=CARTESIAN_POINT('Ctrl Pts',(1.0852948664173,-0.105373203004237,2.68068203601616));
#7951=CARTESIAN_POINT('Ctrl Pts',(1.00539530848997,0.426480980519131,2.70851510392812));
#7952=CARTESIAN_POINT('Ctrl Pts',(0.679609573339881,0.857002336026301,2.7363888804944));
#7953=CARTESIAN_POINT('Ctrl Pts',(0.242228396206659,1.05406947259606,2.76120094819001));
#7954=CARTESIAN_POINT('Ctrl Pts',(-0.289433825273236,1.05900157503401,2.78914691397882));
#7955=CARTESIAN_POINT('Ctrl Pts',(-0.861030373991185,0.756502517113054,
2.82179513727801));
#7956=CARTESIAN_POINT('Ctrl Pts',(-1.15948386741598,-0.00245881106342116,
2.8622922968233));
#7957=CARTESIAN_POINT('Ctrl Pts',(-0.849819252545902,-0.791606149879273,
2.9044266522989));
#7958=CARTESIAN_POINT('Ctrl Pts',(-0.0848273064559805,-1.16047682132822,
2.94663705560064));
#7959=CARTESIAN_POINT('Ctrl Pts',(0.728338616139595,-0.909963609903424,
2.98891980674896));
#7960=CARTESIAN_POINT('Ctrl Pts',(1.15452570093491,-0.172022292800125,3.03127110274204));
#7961=CARTESIAN_POINT('Ctrl Pts',(0.965079959728901,0.659906484623926,3.07368702284038));
#7962=CARTESIAN_POINT('Ctrl Pts',(0.258512451458961,1.14196808324737,3.11616354351132));
#7963=CARTESIAN_POINT('Ctrl Pts',(-0.492717397384934,1.02781794268986,3.15397066853381));
#7964=CARTESIAN_POINT('Ctrl Pts',(-0.950847731766782,0.578891230696036,
3.18708578741999));
#7965=CARTESIAN_POINT('Ctrl Pts',(-1.11322603418831,0.0543699563964829,
3.21549214280387));
#7966=CARTESIAN_POINT('Ctrl Pts',(-1.00397682800075,-0.485299668185688,
3.24391918371992));
#7967=CARTESIAN_POINT('Ctrl Pts',(-0.689560596566738,-0.85912025786842,
3.2692049003822));
#7968=CARTESIAN_POINT('Ctrl Pts',(-0.203462101275883,-1.09903917913844,
3.29766639858301));
#7969=CARTESIAN_POINT('Ctrl Pts',(0.296274556510708,-1.07870085350966,3.32298079518316));
#7970=CARTESIAN_POINT('Ctrl Pts',(0.813909810244539,-0.768416856681802,
3.35464092662437));
#7971=CARTESIAN_POINT('Ctrl Pts',(1.10016251506307,-0.282678926353398,3.38314956983213));
#7972=CARTESIAN_POINT('Ctrl Pts',(1.06842542005047,0.330699838209083,3.41484232929802));
#7973=CARTESIAN_POINT('Ctrl Pts',(0.781036889262004,0.801635745996559,3.44337716794684));
#7974=CARTESIAN_POINT('Ctrl Pts',(0.3026681656048,1.07751158150631,3.47192198965488));
#7975=CARTESIAN_POINT('Ctrl Pts',(-0.341977208139237,1.09513778685306,3.5052343169007));
#7976=CARTESIAN_POINT('Ctrl Pts',(-0.975597618652369,0.664760099314692,
3.54331757606612));
#7977=CARTESIAN_POINT('Ctrl Pts',(-1.13429370842399,-0.0357778387848846,
3.57903024860792));
#7978=CARTESIAN_POINT('Ctrl Pts',(-0.952497172320662,-0.550291907933128,
3.60760379990449));
#7979=CARTESIAN_POINT('Ctrl Pts',(-0.68624513734708,-0.860512981218381,
3.62903507783467));
#7980=CARTESIAN_POINT('Ctrl Pts',(-0.324306798008731,-1.0514860754467,3.65046688028005));
#7981=CARTESIAN_POINT('Ctrl Pts',(0.127344232453658,-1.10276625857497,3.674279919598));
#7982=CARTESIAN_POINT('Ctrl Pts',(0.607784221866902,-0.941400265606059,
3.70047332316486));
#7983=CARTESIAN_POINT('Ctrl Pts',(0.983690388895233,-0.535896868540009,
3.72904537472281));
#7984=CARTESIAN_POINT('Ctrl Pts',(1.08731538430027,-0.128732018548745,3.75076902067426));
#7985=CARTESIAN_POINT('Ctrl Pts',(1.06753777509939,0.150334725456009,3.7656464393213));
#7986=CARTESIAN_POINT('Ctrl Pts',(1.02549367550628,0.347236435696266,3.7763575734054));
#7987=CARTESIAN_POINT('Ctrl Pts',(0.880884191480398,0.671592660752369,3.7951003560531));
#7988=CARTESIAN_POINT('Ctrl Pts',(0.491799935626419,1.0196644890383,3.82187027476111));
#7989=CARTESIAN_POINT('Ctrl Pts',(-0.126065746592581,1.12455786056488,3.85398342973913));
#7990=CARTESIAN_POINT('Ctrl Pts',(-0.704583522010695,0.88486307777345,3.88608387297236));
#7991=CARTESIAN_POINT('Ctrl Pts',(-1.06683466983354,0.3742832244399,3.91816964977168));
#7992=CARTESIAN_POINT('Ctrl Pts',(-1.10184933977514,-0.250419432627018,
3.95023881727803));
#7993=CARTESIAN_POINT('Ctrl Pts',(-0.799326718711519,-0.797694380880393,
3.98228945733906));
#7994=CARTESIAN_POINT('Ctrl Pts',(-0.252343111177166,-1.09993153075449,
4.01431965364637));
#7995=CARTESIAN_POINT('Ctrl Pts',(0.371159169345164,-1.06485412373635,4.0463275194738));
#7996=CARTESIAN_POINT('Ctrl Pts',(0.880047504125487,-0.703696890362346,
4.07831118189475));
#7997=CARTESIAN_POINT('Ctrl Pts',(1.11857837754389,-0.127626743256515,4.11026879475596));
#7998=CARTESIAN_POINT('Ctrl Pts',(1.01416153614381,0.486524030990474,4.14219853012843));
#7999=CARTESIAN_POINT('Ctrl Pts',(0.599338058827864,0.950520440175857,4.17409858361638));
#8000=CARTESIAN_POINT('Ctrl Pts',(0.00190308953361062,1.12257447034417,
4.20596718959497));
#8001=CARTESIAN_POINT('Ctrl Pts',(-0.595087816877256,0.950429978912684,
4.23780259148061));
#8002=CARTESIAN_POINT('Ctrl Pts',(-0.992818074176864,0.504960206465758,
4.26842528448615));
#8003=CARTESIAN_POINT('Ctrl Pts',(-1.10558192615926,-0.0535255134762696,
4.29783816996833));
#8004=CARTESIAN_POINT('Ctrl Pts',(-0.944245633155887,-0.574182433998452,
4.326044460862));
#8005=CARTESIAN_POINT('Ctrl Pts',(-0.489615552103502,-1.02023046107543,
4.35891537170686));
#8006=CARTESIAN_POINT('Ctrl Pts',(0.255873406558148,-1.13223620757883,4.39642822383059));
#8007=CARTESIAN_POINT('Ctrl Pts',(0.956585537399415,-0.654531370431507,
4.43855371945495));
#8008=CARTESIAN_POINT('Ctrl Pts',(1.14416456861692,0.170066871142059,4.48059920430672));
#8009=CARTESIAN_POINT('Ctrl Pts',(0.722117099067864,0.901002181388938,4.52256123999552));
#8010=CARTESIAN_POINT('Ctrl Pts',(-0.0838676738781217,1.14921441407926,
4.5644365266184));
#8011=CARTESIAN_POINT('Ctrl Pts',(-0.755677502986392,0.824069849946143,
4.60157908243497));
#8012=CARTESIAN_POINT('Ctrl Pts',(-1.05498104408691,0.271521112381307,4.63401858831428));
#8013=CARTESIAN_POINT('Ctrl Pts',(-1.05483403133078,-0.26522135570406,4.66178172056988));
#8014=CARTESIAN_POINT('Ctrl Pts',(-0.79840547489227,-0.736599185468657,
4.68950186792131));
#8015=CARTESIAN_POINT('Ctrl Pts',(-0.3483499377511,-1.02663834291108,4.71717822726345));
#8016=CARTESIAN_POINT('Ctrl Pts',(0.184757632451299,-1.06688722115596,4.74481003558103));
#8017=CARTESIAN_POINT('Ctrl Pts',(0.600256695779753,-0.878980608467174,
4.7683735201888));
#8018=CARTESIAN_POINT('Ctrl Pts',(0.853850233649786,-0.610120445383555,
4.78788851920089));
#8019=CARTESIAN_POINT('Ctrl Pts',(1.03381570897682,-0.262894148472765,4.80853189587555));
#8020=CARTESIAN_POINT('Ctrl Pts',(1.06215687349528,0.238874309450968,4.83429913779336));
#8021=CARTESIAN_POINT('Ctrl Pts',(0.770634803840811,0.765869068483215,4.86515976481244));
#8022=CARTESIAN_POINT('Ctrl Pts',(0.244684747552399,1.05635550605388,4.89595947659513));
#8023=CARTESIAN_POINT('Ctrl Pts',(-0.354100647382748,1.02257824395859,4.92669748292077));
#8024=CARTESIAN_POINT('Ctrl Pts',(-0.842095960257555,0.676096127224308,
4.95737304397893));
#8025=CARTESIAN_POINT('Ctrl Pts',(-1.07050216965279,0.124232350128257,4.98798547954758));
#8026=CARTESIAN_POINT('Ctrl Pts',(-0.970487698233666,-0.463339790807337,
5.01853416178037));
#8027=CARTESIAN_POINT('Ctrl Pts',(-0.57403535125674,-0.906703305752076,
5.04901852189829));
#8028=CARTESIAN_POINT('Ctrl Pts',(-0.00367933936324437,-1.07083384017741,
5.07943804916124));
#8029=CARTESIAN_POINT('Ctrl Pts',(0.56535226719551,-0.906710964597204,5.10979228847672));
#8030=CARTESIAN_POINT('Ctrl Pts',(0.95899197878984,-0.465956326824321,5.14008084401914));
#8031=CARTESIAN_POINT('Ctrl Pts',(1.05758360680831,0.115400410376887,5.17030337915801));
#8032=CARTESIAN_POINT('Ctrl Pts',(0.832257130959616,0.658907139635372,5.20045961311858));
#8033=CARTESIAN_POINT('Ctrl Pts',(0.353362036446966,0.998475173781019,5.23054933034559));
#8034=CARTESIAN_POINT('Ctrl Pts',(-0.231493376683462,1.03113233690688,5.26057235733975));
#8035=CARTESIAN_POINT('Ctrl Pts',(-0.742941371583914,0.748253733713579,
5.29052861685377));
#8036=CARTESIAN_POINT('Ctrl Pts',(-1.02486870130036,0.23775759542928,5.3204180022368));
#8037=CARTESIAN_POINT('Ctrl Pts',(-0.992064317380329,-0.343173817499407,
5.3502406538254));
#8038=CARTESIAN_POINT('Ctrl Pts',(-0.655975229859479,-0.81659286891466,
5.37999633599993));
#8039=CARTESIAN_POINT('Ctrl Pts',(-0.120753665413257,-1.03807600951265,
5.40968580999697));
#8040=CARTESIAN_POINT('Ctrl Pts',(0.44897427078276,-0.941278849111864,5.43930775328404));
#8041=CARTESIAN_POINT('Ctrl Pts',(0.878820594563222,-0.556707495126734,
5.46886560818098));
#8042=CARTESIAN_POINT('Ctrl Pts',(0.984806813297395,-0.188706783169536,
5.48852259094232));
#8043=CARTESIAN_POINT('Ctrl Pts',(0.984831692610592,-0.00389691057600537,
5.49834668730695));
#8044=CARTESIAN_POINT('Ctrl Pts',(0.97755951672157,0.00397819713203481,
2.00010574185718));
#8045=CARTESIAN_POINT('Ctrl Pts',(0.977534817777559,0.1874482168994,2.009858614518));
#8046=CARTESIAN_POINT('Ctrl Pts',(0.872339507129369,0.552742035957965,2.02937002260745));
#8047=CARTESIAN_POINT('Ctrl Pts',(0.445612976498857,0.934542787186617,2.05871357126365));
#8048=CARTESIAN_POINT('Ctrl Pts',(-0.120030718543652,1.03065208177895,2.08812225036493));
#8049=CARTESIAN_POINT('Ctrl Pts',(-0.651468641058004,0.81074656763505,2.11760084182634));
#8050=CARTESIAN_POINT('Ctrl Pts',(-0.985218541716035,0.340638135385857,
2.14714764844481));
#8051=CARTESIAN_POINT('Ctrl Pts',(-1.01780770850236,-0.236290452249486,
2.1767638465366));
#8052=CARTESIAN_POINT('Ctrl Pts',(-0.737804384439041,-0.743333134894278,
2.20644924954275));
#8053=CARTESIAN_POINT('Ctrl Pts',(-0.229775908433837,-1.02432739723473,
2.23620424753441));
#8054=CARTESIAN_POINT('Ctrl Pts',(0.351236203556259,-0.991916639617009,
2.26602880347846));
#8055=CARTESIAN_POINT('Ctrl Pts',(0.827059185578202,-0.654513807733518,
2.29592316173363));
#8056=CARTESIAN_POINT('Ctrl Pts',(1.05094913773538,-0.114539223746344,2.32588691927782));
#8057=CARTESIAN_POINT('Ctrl Pts',(0.953019218248555,0.463396416555815,2.35592076218885));
#8058=CARTESIAN_POINT('Ctrl Pts',(0.626882081793141,0.828092290475244,2.3810056356548));
#8059=CARTESIAN_POINT('Ctrl Pts',(0.279001515164431,0.98329371752799,2.40111022029383));
#8060=CARTESIAN_POINT('Ctrl Pts',(-0.00404384991316098,1.02341077763893,
2.41620568810213));
#8061=CARTESIAN_POINT('Ctrl Pts',(-0.287527493131225,0.983358922547369,
2.43131843531318));
#8062=CARTESIAN_POINT('Ctrl Pts',(-0.549169823355069,0.866360638694792,
2.44644850402512));
#8063=CARTESIAN_POINT('Ctrl Pts',(-0.768302851844728,0.681237070886304,
2.46159552744086));
#8064=CARTESIAN_POINT('Ctrl Pts',(-0.969606942749099,0.380577490179153,
2.48069205537781));
#8065=CARTESIAN_POINT('Ctrl Pts',(-1.04090110132001,0.0287889134734739,
2.49925258741977));
#8066=CARTESIAN_POINT('Ctrl Pts',(-0.981332549271593,-0.306846625190479,
2.51728108741502));
#8067=CARTESIAN_POINT('Ctrl Pts',(-0.841439122236331,-0.617828920196817,
2.53532696806566));
#8068=CARTESIAN_POINT('Ctrl Pts',(-0.528617679054796,-0.923413568511115,
2.55791563566096));
#8069=CARTESIAN_POINT('Ctrl Pts',(-0.0792029712632743,-1.04963369664941,
2.5820592733512));
#8070=CARTESIAN_POINT('Ctrl Pts',(0.433613375636684,-0.977259413861191,
2.60926626333433));
#8071=CARTESIAN_POINT('Ctrl Pts',(0.86691020025717,-0.656268692809005,2.63652289720304));
#8072=CARTESIAN_POINT('Ctrl Pts',(1.06712276644286,-0.102855375409246,2.66687533427124));
#8073=CARTESIAN_POINT('Ctrl Pts',(0.98857794766632,0.420176175347904,2.69424420831848));
#8074=CARTESIAN_POINT('Ctrl Pts',(0.668088783928289,0.84372911958199,2.72166407525147));
#8075=CARTESIAN_POINT('Ctrl Pts',(0.237626170167846,1.03771059246847,2.74608285338797));
#8076=CARTESIAN_POINT('Ctrl Pts',(-0.285834074724791,1.0425713500964,2.77359680577556));
#8077=CARTESIAN_POINT('Ctrl Pts',(-0.848855562512735,0.744685054006121,
2.80575161465571));
#8078=CARTESIAN_POINT('Ctrl Pts',(-1.14307267505854,-0.00325442246706518,
2.8456576200506));
#8079=CARTESIAN_POINT('Ctrl Pts',(-0.837781318697799,-0.781552909693705,
2.88720708486476));
#8080=CARTESIAN_POINT('Ctrl Pts',(-0.0828721428173334,-1.14567971574881,
2.92885934862034));
#8081=CARTESIAN_POINT('Ctrl Pts',(0.720219591828141,-0.898389153408221,
2.97061256607032));
#8082=CARTESIAN_POINT('Ctrl Pts',(1.14151252862521,-0.169156474837318,3.01246340210315));
#8083=CARTESIAN_POINT('Ctrl Pts',(0.954270451079617,0.653649229724285,3.05440814190739));
#8084=CARTESIAN_POINT('Ctrl Pts',(0.255025659690968,1.13086513577111,3.09644483636185));
#8085=CARTESIAN_POINT('Ctrl Pts',(-0.489061511145333,1.01792230474927,3.1338859178981));
#8086=CARTESIAN_POINT('Ctrl Pts',(-0.943166447988804,0.572999920918024,
3.1667058728693));
#8087=CARTESIAN_POINT('Ctrl Pts',(-1.10422957591935,0.0528956969736171,
3.19486998840399));
#8088=CARTESIAN_POINT('Ctrl Pts',(-0.99585841718268,-0.482570482219919,
3.22307483505779));
#8089=CARTESIAN_POINT('Ctrl Pts',(-0.68379925456048,-0.853657824468507,
3.24816978426164));
#8090=CARTESIAN_POINT('Ctrl Pts',(-0.201021562509179,-1.09194860971787,
3.27643689660237));
#8091=CARTESIAN_POINT('Ctrl Pts',(0.295507073604264,-1.07180490446086,3.3015851015371));
#8092=CARTESIAN_POINT('Ctrl Pts',(0.810140242218131,-0.763341809894584,
3.33305898227309));
#8093=CARTESIAN_POINT('Ctrl Pts',(1.09493646689165,-0.280204938812027,3.36141446000882));
#8094=CARTESIAN_POINT('Ctrl Pts',(1.06338198271354,0.330333565929847,3.39295813889907));
#8095=CARTESIAN_POINT('Ctrl Pts',(0.777210322504459,0.799346590189962,3.42137245074107));
#8096=CARTESIAN_POINT('Ctrl Pts',(0.300565645225493,1.0742632068725,3.44981223300455));
#8097=CARTESIAN_POINT('Ctrl Pts',(-0.342137134487029,1.09188368707827,3.48302128705105));
#8098=CARTESIAN_POINT('Ctrl Pts',(-0.974318785413307,0.662612446779102,
3.52100929419482));
#8099=CARTESIAN_POINT('Ctrl Pts',(-1.13288648807811,-0.0368107892008958,
3.55666065886606));
#8100=CARTESIAN_POINT('Ctrl Pts',(-0.951263764107293,-0.550894470418624,
3.58520750931815));
#8101=CARTESIAN_POINT('Ctrl Pts',(-0.685143524722543,-0.860992717462809,
3.60662854664387));
#8102=CARTESIAN_POINT('Ctrl Pts',(-0.323240816819056,-1.05196957863857,
3.62805661151224));
#8103=CARTESIAN_POINT('Ctrl Pts',(0.128560007356371,-1.10328952951889,3.65187603774534));
#8104=CARTESIAN_POINT('Ctrl Pts',(0.609407280723653,-0.941828387728985,
3.67808837863482));
#8105=CARTESIAN_POINT('Ctrl Pts',(0.98586930660155,-0.535768218197723,3.70670010871054));
#8106=CARTESIAN_POINT('Ctrl Pts',(1.0897063480334,-0.127854204552833,3.72846073180296));
#8107=CARTESIAN_POINT('Ctrl Pts',(1.06988164984646,0.15186778414323,3.74337260693928));
#8108=CARTESIAN_POINT('Ctrl Pts',(1.02773317276792,0.34926212253662,3.75411020888856));
#8109=CARTESIAN_POINT('Ctrl Pts',(0.882741007204007,0.674496884799054,3.77290255357357));
#8110=CARTESIAN_POINT('Ctrl Pts',(0.492481996563103,1.02367766444837,3.79975197771051));
#8111=CARTESIAN_POINT('Ctrl Pts',(-0.127690565781102,1.12901692327556,3.8319825979689));
#8112=CARTESIAN_POINT('Ctrl Pts',(-0.708748153845812,0.888319810350649,
3.86421960143728));
#8113=CARTESIAN_POINT('Ctrl Pts',(-1.07284204822087,0.37523040851078,3.89646195079746));
#8114=CARTESIAN_POINT('Ctrl Pts',(-1.10810231534743,-0.252955497845161,
3.92870698364651));
#8115=CARTESIAN_POINT('Ctrl Pts',(-0.803754630503077,-0.803637553165077,
3.96095281863656));
#8116=CARTESIAN_POINT('Ctrl Pts',(-0.253088561756074,-1.10796766192506,
3.99319723942644));
#8117=CARTESIAN_POINT('Ctrl Pts',(0.375010957528947,-1.07268207150159,4.02543819894899));
#8118=CARTESIAN_POINT('Ctrl Pts',(0.887976540139475,-0.708692354908092,
4.05767359098646));
#8119=CARTESIAN_POINT('Ctrl Pts',(1.12858897297226,-0.127723402477217,4.08990133451333));
#8120=CARTESIAN_POINT('Ctrl Pts',(1.02326898300414,0.492031189427128,4.12211937335469));
#8121=CARTESIAN_POINT('Ctrl Pts',(0.604466062779254,0.960551404367795,4.15432557540022));
#8122=CARTESIAN_POINT('Ctrl Pts',(0.000927783036573728,1.13441322120194,
4.18651801173377));
#8123=CARTESIAN_POINT('Ctrl Pts',(-0.602520120716071,0.960458611226862,
4.21869431046299));
#8124=CARTESIAN_POINT('Ctrl Pts',(-1.00478741507514,0.509967747015279,4.24966196687484));
#8125=CARTESIAN_POINT('Ctrl Pts',(-1.11892334048673,-0.0551203638852278,
4.27942038227802));
#8126=CARTESIAN_POINT('Ctrl Pts',(-0.955613823551837,-0.582210419872125,
4.30797396885712));
#8127=CARTESIAN_POINT('Ctrl Pts',(-0.495204396789493,-1.03399629100515,
4.34126381542087));
#8128=CARTESIAN_POINT('Ctrl Pts',(0.2602289300512,-1.14757077870588,4.37927522482165));
#8129=CARTESIAN_POINT('Ctrl Pts',(0.970816206161694,-0.663265764508169,
4.42198822284881));
#8130=CARTESIAN_POINT('Ctrl Pts',(1.1612353098011,0.173412559077483,4.46464709152681));
#8131=CARTESIAN_POINT('Ctrl Pts',(0.73281467250382,0.915574596057104,4.50724834203436));
#8132=CARTESIAN_POINT('Ctrl Pts',(-0.085964988811639,1.16782799270487,4.54978699118941));
#8133=CARTESIAN_POINT('Ctrl Pts',(-0.768880602583059,0.837392966288513,
4.58753928679426));
#8134=CARTESIAN_POINT('Ctrl Pts',(-1.07329276575036,0.275486454169533,4.62052734960056));
#8135=CARTESIAN_POINT('Ctrl Pts',(-1.07316083376288,-0.27056471925353,4.64877133408048));
#8136=CARTESIAN_POINT('Ctrl Pts',(-0.812223242657351,-0.750291341226326,
4.67698085025682));
#8137=CARTESIAN_POINT('Ctrl Pts',(-0.354063516147758,-1.04557309377014,
4.70515509535978));
#8138=CARTESIAN_POINT('Ctrl Pts',(0.188835848046625,-1.08658576479028,4.73329424506581));
#8139=CARTESIAN_POINT('Ctrl Pts',(0.612091477193082,-0.89518184092728,4.75729595235333));
#8140=CARTESIAN_POINT('Ctrl Pts',(0.87049090381391,-0.621232336099561,4.77718028775068));
#8141=CARTESIAN_POINT('Ctrl Pts',(1.05389711917837,-0.267373370743659,4.79821770027757));
#8142=CARTESIAN_POINT('Ctrl Pts',(1.0828048480663,0.2440947028953,4.82448212353492));
#8143=CARTESIAN_POINT('Ctrl Pts',(0.785570688143936,0.781464268917798,4.85594880718113));
#8144=CARTESIAN_POINT('Ctrl Pts',(0.249128587108361,1.07776823295182,4.88736261138121));
#8145=CARTESIAN_POINT('Ctrl Pts',(-0.361785836370703,1.04332703153431,4.91872252432293));
#8146=CARTESIAN_POINT('Ctrl Pts',(-0.859808049698745,0.689748559723978,
4.95002707792092));
#8147=CARTESIAN_POINT('Ctrl Pts',(-1.09297615308804,0.126424919553853,4.98127509388506));
#8148=CARTESIAN_POINT('Ctrl Pts',(-0.990875767219502,-0.47349721224129,
5.0124653393971));
#8149=CARTESIAN_POINT('Ctrl Pts',(-0.586016424119173,-0.926284211843029,
5.04359668436538));
#8150=CARTESIAN_POINT('Ctrl Pts',(-0.00343903085660042,-1.09394513826332,
5.07466803457235));
#8151=CARTESIAN_POINT('Ctrl Pts',(0.57789653224993,-0.926285315052589,5.10567835345191));
#8152=CARTESIAN_POINT('Ctrl Pts',(0.9801178138107,-0.475936671342823,5.13662665912829));
#8153=CARTESIAN_POINT('Ctrl Pts',(1.08087952050974,0.118166939826646,5.16751202559587));
#8154=CARTESIAN_POINT('Ctrl Pts',(0.850589387397783,0.673663880453797,5.19833358312002));
#8155=CARTESIAN_POINT('Ctrl Pts',(0.361082693325379,1.02076245584766,5.22909051751435));
#8156=CARTESIAN_POINT('Ctrl Pts',(-0.236787832380174,1.05414991601765,5.2597820690211));
#8157=CARTESIAN_POINT('Ctrl Pts',(-0.759654102884898,0.764957789837657,
5.29040754589614));
#8158=CARTESIAN_POINT('Ctrl Pts',(-1.0478890117056,0.243040084360927,5.32096628655212));
#8159=CARTESIAN_POINT('Ctrl Pts',(-1.01434736252641,-0.350907601135237,
5.35145773998857));
#8160=CARTESIAN_POINT('Ctrl Pts',(-0.670720080533004,-0.834934758998085,
5.38188128530446));
#8161=CARTESIAN_POINT('Ctrl Pts',(-0.123502010424964,-1.06137898572475,
5.41223662280484));
#8162=CARTESIAN_POINT('Ctrl Pts',(0.458979922580301,-0.962399495397908,
5.44252287745861));
#8163=CARTESIAN_POINT('Ctrl Pts',(0.898423965887827,-0.569251854562554,
5.4727405859251));
#8164=CARTESIAN_POINT('Ctrl Pts',(1.00678249531561,-0.193014045740111,5.49283838071418));
#8165=CARTESIAN_POINT('Ctrl Pts',(1.0068079216488,-0.0041407693603704,5.50287847890709));
#8166=CARTESIAN_POINT('Ctrl Pts',(0.932826886418256,0.00283195947158155,
2.02155536031992));
#8167=CARTESIAN_POINT('Ctrl Pts',(0.932803305353409,0.177998089311277,2.03086681600614));
#8168=CARTESIAN_POINT('Ctrl Pts',(0.832416926289886,0.526449355831317,2.04947889674723));
#8169=CARTESIAN_POINT('Ctrl Pts',(0.425462368210857,0.890529450601189,2.07746218207928));
#8170=CARTESIAN_POINT('Ctrl Pts',(-0.113680331421872,0.982080962129939,
2.10549185328996));
#8171=CARTESIAN_POINT('Ctrl Pts',(-0.619976540307357,0.772544065442153,
2.13357682839298));
#8172=CARTESIAN_POINT('Ctrl Pts',(-0.937793676005252,0.324817811790029,
2.1617153597137));
#8173=CARTESIAN_POINT('Ctrl Pts',(-0.968789729919569,-0.224425204758645,
2.18991046480974));
#8174=CARTESIAN_POINT('Ctrl Pts',(-0.702281633273633,-0.706978147903316,
2.21816297555692));
#8175=CARTESIAN_POINT('Ctrl Pts',(-0.218891386755124,-0.974319694873083,
2.24647466346303));
#8176=CARTESIAN_POINT('Ctrl Pts',(0.333814568943781,-0.943469504346031,
2.27484678113967));
#8177=CARTESIAN_POINT('Ctrl Pts',(0.786375647775339,-0.62254316688173,2.30328080747615));
#8178=CARTESIAN_POINT('Ctrl Pts',(0.999287584601159,-0.109010364379432,
2.33177786821182));
#8179=CARTESIAN_POINT('Ctrl Pts',(0.906153001363644,0.440580406885506,2.36033953197038));
#8180=CARTESIAN_POINT('Ctrl Pts',(0.596008350255508,0.787384121518291,2.3841950831244));
#8181=CARTESIAN_POINT('Ctrl Pts',(0.26519405894642,0.934970553828525,2.40331371530758));
#8182=CARTESIAN_POINT('Ctrl Pts',(-0.00397354741378065,0.973119533744013,
2.41766940006373));
#8183=CARTESIAN_POINT('Ctrl Pts',(-0.273566744652249,0.93502873494253,2.43204204909921));
#8184=CARTESIAN_POINT('Ctrl Pts',(-0.522400248336806,0.823757746325111,
2.4464318017068));
#8185=CARTESIAN_POINT('Ctrl Pts',(-0.730817383368411,0.647684837741542,
2.46083869981358));
#8186=CARTESIAN_POINT('Ctrl Pts',(-0.922289399192392,0.36171191420862,2.47900280186383));
#8187=CARTESIAN_POINT('Ctrl Pts',(-0.990115280771857,0.0270487089396692,
2.49666133821441));
#8188=CARTESIAN_POINT('Ctrl Pts',(-0.93344377138001,-0.29226896767037,2.51381363816868));
#8189=CARTESIAN_POINT('Ctrl Pts',(-0.800338308713536,-0.588160741791901,
2.53098451463937));
#8190=CARTESIAN_POINT('Ctrl Pts',(-0.502644742748064,-0.878987021396976,
2.55248281477416));
#8191=CARTESIAN_POINT('Ctrl Pts',(-0.0748628151458846,-0.999136993401524,
2.57546548511536));
#8192=CARTESIAN_POINT('Ctrl Pts',(0.413375452637366,-0.930246526757298,
2.60136908260148));
#8193=CARTESIAN_POINT('Ctrl Pts',(0.826056853037204,-0.624555315394363,
2.62733007231111));
#8194=CARTESIAN_POINT('Ctrl Pts',(1.0168419590957,-0.0972852674529773,2.65625128192227));
#8195=CARTESIAN_POINT('Ctrl Pts',(0.941995491232734,0.40123528872719,2.68233928665076));
#8196=CARTESIAN_POINT('Ctrl Pts',(0.636429682017026,0.805122864353395,2.70848641485114));
#8197=CARTESIAN_POINT('Ctrl Pts',(0.225807606948362,0.990184376230355,2.7317813313523));
#8198=CARTESIAN_POINT('Ctrl Pts',(-0.27371468395447,0.994843165208457,2.75803796083437));
#8199=CARTESIAN_POINT('Ctrl Pts',(-0.811295562767927,0.710483997877433,
2.78874044098356));
#8200=CARTESIAN_POINT('Ctrl Pts',(-1.09254471947464,-0.00413748468829043,
2.82687585935908));
#8201=CARTESIAN_POINT('Ctrl Pts',(-0.800710019071887,-0.748493642300563,
2.86661399643152));
#8202=CARTESIAN_POINT('Ctrl Pts',(-0.0781674205730973,-1.09716986953638,
2.90648808960406));
#8203=CARTESIAN_POINT('Ctrl Pts',(0.691367439738533,-0.860372850065677,
2.9464982533936));
#8204=CARTESIAN_POINT('Ctrl Pts',(1.09559718621259,-0.160996041341971,2.98664420509449));
#8205=CARTESIAN_POINT('Ctrl Pts',(0.915963771274089,0.629121386204399,3.02692562208008));
#8206=CARTESIAN_POINT('Ctrl Pts',(0.243844124877269,1.08804711068323,3.06734171283987));
#8207=CARTESIAN_POINT('Ctrl Pts',(-0.47240323087623,0.979478908158574,3.10338643967991));
#8208=CARTESIAN_POINT('Ctrl Pts',(-0.910000320002659,0.550829528387608,
3.13501124859862));
#8209=CARTESIAN_POINT('Ctrl Pts',(-1.06536518427627,0.0492471101455223,
3.16217730264769));
#8210=CARTESIAN_POINT('Ctrl Pts',(-0.960838705697807,-0.467598238213527,
3.18940094649933));
#8211=CARTESIAN_POINT('Ctrl Pts',(-0.65934937746825,-0.826164624702505,
3.21365194639263));
#8212=CARTESIAN_POINT('Ctrl Pts',(-0.192619566100375,-1.05658204389069,
3.24098101787109));
#8213=CARTESIAN_POINT('Ctrl Pts',(0.287953883038658,-1.03716173927374,3.26532513654264));
#8214=CARTESIAN_POINT('Ctrl Pts',(0.786515199786917,-0.738387174635933,
3.29581702917111));
#8215=CARTESIAN_POINT('Ctrl Pts',(1.0627682681574,-0.269950457591334,3.32331568948603));
#8216=CARTESIAN_POINT('Ctrl Pts',(1.03222736433692,0.322770007878815,3.35394076194273));
#8217=CARTESIAN_POINT('Ctrl Pts',(0.754172111200573,0.778605651076345,3.38155794876388));
#8218=CARTESIAN_POINT('Ctrl Pts',(0.290513273528267,1.04611740958465,3.40922867610414));
#8219=CARTESIAN_POINT('Ctrl Pts',(-0.335359646284715,1.06336169172191,3.44157258610646));
#8220=CARTESIAN_POINT('Ctrl Pts',(-0.951983941078512,0.644937022856501,
3.4786243719862));
#8221=CARTESIAN_POINT('Ctrl Pts',(-1.10707031340484,-0.0382267088572197,
3.51345595556107));
#8222=CARTESIAN_POINT('Ctrl Pts',(-0.929495283855687,-0.540997199899391,
3.54137565325151));
#8223=CARTESIAN_POINT('Ctrl Pts',(-0.669049818764436,-0.8445166517426,3.56234258200301));
#8224=CARTESIAN_POINT('Ctrl Pts',(-0.314526844233505,-1.03163152300883,
3.58333707155614));
#8225=CARTESIAN_POINT('Ctrl Pts',(0.128448115091551,-1.08197849543191,3.60669360763323));
#8226=CARTESIAN_POINT('Ctrl Pts',(0.60040054697126,-0.923572454548513,3.63242325159083));
#8227=CARTESIAN_POINT('Ctrl Pts',(0.970355718452742,-0.524664964388033,
3.66053639605977));
#8228=CARTESIAN_POINT('Ctrl Pts',(1.07257858888191,-0.123363125148085,3.68194931382862));
#8229=CARTESIAN_POINT('Ctrl Pts',(1.05306973839567,0.15199342992826,3.69662895181969));
#8230=CARTESIAN_POINT('Ctrl Pts',(1.01156739393715,0.346370357112534,3.70720281308074));
#8231=CARTESIAN_POINT('Ctrl Pts',(0.868732331837759,0.666808155110966,3.72571919069949));
#8232=CARTESIAN_POINT('Ctrl Pts',(0.483879628566754,1.01127896449476,3.7522054917375));
#8233=CARTESIAN_POINT('Ctrl Pts',(-0.12857131584191,1.11542778844378,3.78403970128842));
#8234=CARTESIAN_POINT('Ctrl Pts',(-0.703235081453136,0.877515951502692,
3.81592375908098));
#8235=CARTESIAN_POINT('Ctrl Pts',(-1.06387585411653,0.369502985541506,3.84785557289108));
#8236=CARTESIAN_POINT('Ctrl Pts',(-1.09896190148898,-0.253391176953802,
3.87983352293997));
#8237=CARTESIAN_POINT('Ctrl Pts',(-0.796868983409988,-0.800244509653766,
3.91185571127886));
#8238=CARTESIAN_POINT('Ctrl Pts',(-0.249401044438271,-1.10294610857381,
3.94392028721854));
#8239=CARTESIAN_POINT('Ctrl Pts',(0.375981408272009,-1.06793540537711,3.97602532458088));
#8240=CARTESIAN_POINT('Ctrl Pts',(0.887494631104647,-0.705126302172368,
4.00816887101121));
#8241=CARTESIAN_POINT('Ctrl Pts',(1.12783557019956,-0.125133385342958,4.04034894524235));
#8242=CARTESIAN_POINT('Ctrl Pts',(1.02266005657607,0.494501201713791,4.07256351094201));
#8243=CARTESIAN_POINT('Ctrl Pts',(0.603467469596099,0.963639648177038,4.10481055037349));
#8244=CARTESIAN_POINT('Ctrl Pts',(-0.00156042575409069,1.13805630555576,
4.13708792196456));
#8245=CARTESIAN_POINT('Ctrl Pts',(-0.607394163231413,0.963537549874477,
4.16939369795753));
#8246=CARTESIAN_POINT('Ctrl Pts',(-1.01187486453871,0.510748224645048,4.20052792601527));
#8247=CARTESIAN_POINT('Ctrl Pts',(-1.12684783390284,-0.0580425136282725,
4.23048610732755));
#8248=CARTESIAN_POINT('Ctrl Pts',(-0.962363092043994,-0.589239644075659,
4.2592618020737));
#8249=CARTESIAN_POINT('Ctrl Pts',(-0.497901120763859,-1.04513031762221,
4.29285265406363));
#8250=CARTESIAN_POINT('Ctrl Pts',(0.265414780641501,-1.16017299694639,4.33126650928724));
#8251=CARTESIAN_POINT('Ctrl Pts',(0.984906508993433,-0.670147646454155,
4.37450949010921));
#8252=CARTESIAN_POINT('Ctrl Pts',(1.17829785257441,0.178234358754055,4.41777419186001));
#8253=CARTESIAN_POINT('Ctrl Pts',(0.74334096841188,0.932290366300818,4.46105479234514));
#8254=CARTESIAN_POINT('Ctrl Pts',(-0.089749850748141,1.18925176092741,4.50434628274598));
#8255=CARTESIAN_POINT('Ctrl Pts',(-0.785979921194401,0.852637808144917,
4.54283287791217));
#8256=CARTESIAN_POINT('Ctrl Pts',(-1.09678413718196,0.279114855043184,4.57650810802541));
#8257=CARTESIAN_POINT('Ctrl Pts',(-1.09673130021223,-0.278856026110746,
4.60536977372265));
#8258=CARTESIAN_POINT('Ctrl Pts',(-0.829860168431522,-0.769629991342529,
4.63422895110683));
#8259=CARTESIAN_POINT('Ctrl Pts',(-0.360713606530814,-1.07209234198494,
4.66308348222077));
#8260=CARTESIAN_POINT('Ctrl Pts',(0.195822348541668,-1.11420174957979,4.69193058468913));
#8261=CARTESIAN_POINT('Ctrl Pts',(0.630237211031698,-0.917836549559489,
4.71656627824889));
#8262=CARTESIAN_POINT('Ctrl Pts',(0.895633186161231,-0.636491077288054,
4.73698860804468));
#8263=CARTESIAN_POINT('Ctrl Pts',(1.08412177321864,-0.272871489826572,4.75860802443867));
#8264=CARTESIAN_POINT('Ctrl Pts',(1.11394266799808,0.253195431719909,4.78562493558549));
#8265=CARTESIAN_POINT('Ctrl Pts',(0.80797744806265,0.806563226819446,4.81802760839723));
#8266=CARTESIAN_POINT('Ctrl Pts',(0.255057409915322,1.11208766611089,4.85041166201342));
#8267=CARTESIAN_POINT('Ctrl Pts',(-0.375360011406527,1.07664591176693,4.88277443242993));
#8268=CARTESIAN_POINT('Ctrl Pts',(-0.889872436862409,0.711478850433845,
4.91511397615734));
#8269=CARTESIAN_POINT('Ctrl Pts',(-1.13106879693417,0.129004648892796,4.94742804403158));
#8270=CARTESIAN_POINT('Ctrl Pts',(-1.02547541511561,-0.491986465704221,
4.97971454047685));
#8271=CARTESIAN_POINT('Ctrl Pts',(-0.606065844114821,-0.96117968559332,
5.01197132966905));
#8272=CARTESIAN_POINT('Ctrl Pts',(-0.00190792747688937,-1.13514133907331,
5.04419633657574));
#8273=CARTESIAN_POINT('Ctrl Pts',(0.601563511725319,-0.961184874297887,
5.07638748778849));
#8274=CARTESIAN_POINT('Ctrl Pts',(1.01951677311495,-0.493344052857984,5.10854275472083));
#8275=CARTESIAN_POINT('Ctrl Pts',(1.12437206455613,0.124425076160577,5.14066013263499));
#8276=CARTESIAN_POINT('Ctrl Pts',(0.88477473461175,0.702570826283213,5.17273765929341));
#8277=CARTESIAN_POINT('Ctrl Pts',(0.374970578542117,1.06415151415046,5.20477339242679));
#8278=CARTESIAN_POINT('Ctrl Pts',(-0.248216330495147,1.09902333007776,5.23676544866705));
#8279=CARTESIAN_POINT('Ctrl Pts',(-0.79365941366675,0.79742110391797,5.26871194962692));
#8280=CARTESIAN_POINT('Ctrl Pts',(-1.09458936477043,0.252650565010212,5.30061113031637));
#8281=CARTESIAN_POINT('Ctrl Pts',(-1.05961510152497,-0.367758002763614,
5.33246109735404));
#8282=CARTESIAN_POINT('Ctrl Pts',(-0.700502849367933,-0.87369432558995,
5.364260384324));
#8283=CARTESIAN_POINT('Ctrl Pts',(-0.128229042232588,-1.11057117581653,
5.39600672287796));
#8284=CARTESIAN_POINT('Ctrl Pts',(0.4812925884126,-1.00702848710217,5.42769976907791));
#8285=CARTESIAN_POINT('Ctrl Pts',(0.941404086084559,-0.595482393179593,
5.45933506228865));
#8286=CARTESIAN_POINT('Ctrl Pts',(1.05493386550085,-0.201302816156643,5.48039175829747));
#8287=CARTESIAN_POINT('Ctrl Pts',(1.0549604924824,-0.00351081811190388,
5.49090595660125));
#8288=CARTESIAN_POINT('Ctrl Pts',(0.916369847031328,-0.00102349111045756,
2.09404201605622));
#8289=CARTESIAN_POINT('Ctrl Pts',(0.916346688528236,0.171003742848899,2.10318661477118));
#8290=CARTESIAN_POINT('Ctrl Pts',(0.817707835360784,0.512895716711358,2.12145223875872));
#8291=CARTESIAN_POINT('Ctrl Pts',(0.41920029748926,0.869170209238544,2.14884729591622));
#8292=CARTESIAN_POINT('Ctrl Pts',(-0.107422236712015,0.958431037008827,
2.17622676391991));
#8293=CARTESIAN_POINT('Ctrl Pts',(-0.600746857940946,0.754082977371277,
2.20359747278904));
#8294=CARTESIAN_POINT('Ctrl Pts',(-0.909638270891026,0.31865350810529,2.23095959000811));
#8295=CARTESIAN_POINT('Ctrl Pts',(-0.939549502046027,-0.214226424209876,
2.25831630277396));
#8296=CARTESIAN_POINT('Ctrl Pts',(-0.681405678590222,-0.681304517201164,
2.28566947488182));
#8297=CARTESIAN_POINT('Ctrl Pts',(-0.214358534931351,-0.939427406949708,
2.31302155295729));
#8298=CARTESIAN_POINT('Ctrl Pts',(0.318449240362149,-0.909531728351045,
2.34037479460111));
#8299=CARTESIAN_POINT('Ctrl Pts',(0.753742306192684,-0.600663625481568,
2.36773142222178));
#8300=CARTESIAN_POINT('Ctrl Pts',(0.958021262333031,-0.10755669277854,2.39509395663888));
#8301=CARTESIAN_POINT('Ctrl Pts',(0.86863237642743,0.419049362271387,2.4224642099679));
#8302=CARTESIAN_POINT('Ctrl Pts',(0.571920019213654,0.750656867888804,2.44528213440013));
#8303=CARTESIAN_POINT('Ctrl Pts',(0.255980235250472,0.891581369871216,2.46354143837027));
#8304=CARTESIAN_POINT('Ctrl Pts',(-0.000849208062606655,0.927965626989967,
2.47723951301954));
#8305=CARTESIAN_POINT('Ctrl Pts',(-0.25784438103185,0.89163691871115,2.49094127751245));
#8306=CARTESIAN_POINT('Ctrl Pts',(-0.494833212767144,0.785644887369317,
2.50464698245298));
#8307=CARTESIAN_POINT('Ctrl Pts',(-0.693149427962659,0.618083776493324,
2.51835707335789));
#8308=CARTESIAN_POINT('Ctrl Pts',(-0.875173939491225,0.346184871151078,
2.53562686428944));
#8309=CARTESIAN_POINT('Ctrl Pts',(-0.939531665887204,0.0283479115925304,
2.55239869309082));
#8310=CARTESIAN_POINT('Ctrl Pts',(-0.885762312197225,-0.274533729571816,
2.56866880276681));
#8311=CARTESIAN_POINT('Ctrl Pts',(-0.759584016300259,-0.554994827188533,
2.58494500387052));
#8312=CARTESIAN_POINT('Ctrl Pts',(-0.477657541151781,-0.830327440363872,
2.60530275038326));
#8313=CARTESIAN_POINT('Ctrl Pts',(-0.0731616141952735,-0.943861317503134,
2.62703429354313));
#8314=CARTESIAN_POINT('Ctrl Pts',(0.387950369948457,-0.878766091763475,
2.65149944922312));
#8315=CARTESIAN_POINT('Ctrl Pts',(0.777131349534,-0.590316605789316,2.67598803187672));
#8316=CARTESIAN_POINT('Ctrl Pts',(0.956739044025989,-0.0936873461534193,
2.70322901261928));
#8317=CARTESIAN_POINT('Ctrl Pts',(0.8862663494043,0.37526617083507,2.727771384829));
#8318=CARTESIAN_POINT('Ctrl Pts',(0.599098926797975,0.754728897718691,2.75234086323461));
#8319=CARTESIAN_POINT('Ctrl Pts',(0.21368090376234,0.928370361438052,2.77420537437644));
#8320=CARTESIAN_POINT('Ctrl Pts',(-0.254738122925511,0.93271452307593,2.79882743681787));
#8321=CARTESIAN_POINT('Ctrl Pts',(-0.75828727827768,0.666216656617621,2.82758989707073));
#8322=CARTESIAN_POINT('Ctrl Pts',(-1.02123564536619,-0.00240116619232516,
2.86326862539798));
#8323=CARTESIAN_POINT('Ctrl Pts',(-0.748415847817779,-0.697780968165656,
2.90039680552695));
#8324=CARTESIAN_POINT('Ctrl Pts',(-0.07409131528767,-1.02301638245004,2.93760761266815));
#8325=CARTESIAN_POINT('Ctrl Pts',(0.643203902256486,-0.802146148193398,
2.97490493232259));
#8326=CARTESIAN_POINT('Ctrl Pts',(1.01954723631622,-0.150769416767172,3.01229302565354));
#8327=CARTESIAN_POINT('Ctrl Pts',(0.852292508225827,0.584414907128488,3.04977591907635));
#8328=CARTESIAN_POINT('Ctrl Pts',(0.227276839423578,1.0110674650509,3.08735720401155));
#8329=CARTESIAN_POINT('Ctrl Pts',(-0.438319541939116,0.910113738470391,
3.12085411505228));
#8330=CARTESIAN_POINT('Ctrl Pts',(-0.844801512336328,0.511916553688642,
3.15023160268429));
#8331=CARTESIAN_POINT('Ctrl Pts',(-0.989077176791191,0.0460945198815799,
3.17546084042722));
#8332=CARTESIAN_POINT('Ctrl Pts',(-0.892014438447379,-0.433794636537154,
3.2007381352498));
#8333=CARTESIAN_POINT('Ctrl Pts',(-0.612118438007755,-0.766673921756164,
3.22325206561452));
#8334=CARTESIAN_POINT('Ctrl Pts',(-0.178857765623275,-0.980565792531451,
3.24862139375817));
#8335=CARTESIAN_POINT('Ctrl Pts',(0.267228106207802,-0.962539184921591,
3.27121838614417));
#8336=CARTESIAN_POINT('Ctrl Pts',(0.730013939585809,-0.685206821667964,
3.29952225272199));
#8337=CARTESIAN_POINT('Ctrl Pts',(0.986464765139846,-0.250369071743527,
3.32504870915495));
#8338=CARTESIAN_POINT('Ctrl Pts',(0.95812182499081,0.299918184836265,3.35348122127316));
#8339=CARTESIAN_POINT('Ctrl Pts',(0.69994234794655,0.723197169461558,3.37912524154526));
#8340=CARTESIAN_POINT('Ctrl Pts',(0.26932018482604,0.971666495969792,3.40482455316389));
#8341=CARTESIAN_POINT('Ctrl Pts',(-0.31212188900552,0.98771052697221,3.43487218195244));
#8342=CARTESIAN_POINT('Ctrl Pts',(-0.885238845826609,0.598894963282439,
3.46930673479697));
#8343=CARTESIAN_POINT('Ctrl Pts',(-1.02953961553121,-0.0363787851602884,
3.5016965523722));
#8344=CARTESIAN_POINT('Ctrl Pts',(-0.864336764959382,-0.504181293959062,
3.52767346931298));
#8345=CARTESIAN_POINT('Ctrl Pts',(-0.621930095431672,-0.786700433736122,
3.54718892278537));
#8346=CARTESIAN_POINT('Ctrl Pts',(-0.291824674843086,-0.960947772200679,
3.56673743356965));
#8347=CARTESIAN_POINT('Ctrl Pts',(0.120824733563513,-1.00786799696591,3.58849479474554));
#8348=CARTESIAN_POINT('Ctrl Pts',(0.560718250558898,-0.860264176152269,
3.61247534427901));
#8349=CARTESIAN_POINT('Ctrl Pts',(0.90579561929086,-0.488243207438898,3.63869541996055));
#8350=CARTESIAN_POINT('Ctrl Pts',(1.00123268399749,-0.113720390961006,3.65867897605182));
#8351=CARTESIAN_POINT('Ctrl Pts',(0.983017585188276,0.143402603591866,3.67238638521822));
#8352=CARTESIAN_POINT('Ctrl Pts',(0.944256590238532,0.324946829770906,3.68226204628741));
#8353=CARTESIAN_POINT('Ctrl Pts',(0.810820991239849,0.624325964678426,3.69956105418397));
#8354=CARTESIAN_POINT('Ctrl Pts',(0.451074214704145,0.946410697051131,3.72432137261343));
#8355=CARTESIAN_POINT('Ctrl Pts',(-0.12202991938042,1.04395262161911,3.75411010316036));
#8356=CARTESIAN_POINT('Ctrl Pts',(-0.660359762621321,0.821174393840838,
3.78397519806004));
#8357=CARTESIAN_POINT('Ctrl Pts',(-0.998609248217651,0.344859144986669,
3.8139167304214));
#8358=CARTESIAN_POINT('Ctrl Pts',(-1.03164097244784,-0.239875733016347,
3.84393465319117));
#8359=CARTESIAN_POINT('Ctrl Pts',(-0.747811121324658,-0.753874860605696,
3.8740288769748));
#8360=CARTESIAN_POINT('Ctrl Pts',(-0.232712138351297,-1.03879805778991,
3.90419923342449));
#8361=CARTESIAN_POINT('Ctrl Pts',(0.356495892757353,-1.00592070547447,3.9344454910798));
#8362=CARTESIAN_POINT('Ctrl Pts',(0.839107848540948,-0.663748333283532,
3.96476735078991));
#8363=CARTESIAN_POINT('Ctrl Pts',(1.06625077284666,-0.115907777840236,3.99516444147537));
#8364=CARTESIAN_POINT('Ctrl Pts',(0.966878330006049,0.470257402286813,4.02563633586024));
#8365=CARTESIAN_POINT('Ctrl Pts',(0.569866293499877,0.914758605400251,4.05618251087602));
#8366=CARTESIAN_POINT('Ctrl Pts',(-0.00408784481252405,1.08035069145649,
4.08680243863468));
#8367=CARTESIAN_POINT('Ctrl Pts',(-0.579750345963528,0.914663327800101,
4.11749538541984));
#8368=CARTESIAN_POINT('Ctrl Pts',(-0.964749041164902,0.483870415823376,
4.14712137732599));
#8369=CARTESIAN_POINT('Ctrl Pts',(-1.0744299924881,-0.0581826966804888,
4.17567030962805));
#8370=CARTESIAN_POINT('Ctrl Pts',(-0.917518259249771,-0.565200962277581,
4.2031340732151));
#8371=CARTESIAN_POINT('Ctrl Pts',(-0.473682144476704,-1.00103453406579,
4.23523938847692));
#8372=CARTESIAN_POINT('Ctrl Pts',(0.257222988296793,-1.11148785556699,4.27202226579617));
#8373=CARTESIAN_POINT('Ctrl Pts',(0.947986891210012,-0.641485758789489,
4.31352348095811));
#8374=CARTESIAN_POINT('Ctrl Pts',(1.13439835811232,0.174626964839297,4.35514289607299));
#8375=CARTESIAN_POINT('Ctrl Pts',(0.715278455463992,0.901996673495511,4.3968779276954));
#8376=CARTESIAN_POINT('Ctrl Pts',(-0.0899753508703297,1.15079804708479,
4.43872545034349));
#8377=CARTESIAN_POINT('Ctrl Pts',(-0.764860835418986,0.824889245468528,
4.47602022241449));
#8378=CARTESIAN_POINT('Ctrl Pts',(-1.06684896287779,0.26796150264565,4.50872224677515));
#8379=CARTESIAN_POINT('Ctrl Pts',(-1.0669019032667,-0.274863137816934,4.5367995180593));
#8380=CARTESIAN_POINT('Ctrl Pts',(-0.806952932018616,-0.75318333934492,
4.56492138454683));
#8381=CARTESIAN_POINT('Ctrl Pts',(-0.349034088477564,-1.04854060213485,
4.59308718022527));
#8382=CARTESIAN_POINT('Ctrl Pts',(0.195199242947889,-1.08984580813762,4.62129657098129));
#8383=CARTESIAN_POINT('Ctrl Pts',(0.620780261672434,-0.897578145268399,
4.64542615597834));
#8384=CARTESIAN_POINT('Ctrl Pts',(0.881157012154678,-0.621593420716843,
4.66545991481029));
#8385=CARTESIAN_POINT('Ctrl Pts',(1.06627072006747,-0.264543937473019,4.68668883949075));
#8386=CARTESIAN_POINT('Ctrl Pts',(1.09573971133967,0.252780133526497,4.71325480051859));
#8387=CARTESIAN_POINT('Ctrl Pts',(0.794394693978023,0.798163977577909,4.74518261070608));
#8388=CARTESIAN_POINT('Ctrl Pts',(0.248519420266219,1.09999436085071,4.77715633733294));
#8389=CARTESIAN_POINT('Ctrl Pts',(-0.375240449586358,1.06510654881083,4.80917449611883));
#8390=CARTESIAN_POINT('Ctrl Pts',(-0.885457074079279,0.703208795097844,
4.84123501597506));
#8391=CARTESIAN_POINT('Ctrl Pts',(-1.12524810993215,0.124601555468318,4.87333605018736));
#8392=CARTESIAN_POINT('Ctrl Pts',(-1.02030690402006,-0.493639120147483,
4.90547560083362));
#8393=CARTESIAN_POINT('Ctrl Pts',(-0.602052162605231,-0.961813726065453,
4.93765169075804));
#8394=CARTESIAN_POINT('Ctrl Pts',(0.00182870667745636,-1.135885393394,4.9698622965679));
#8395=CARTESIAN_POINT('Ctrl Pts',(0.606367058350047,-0.961811168634456,
5.00210536221374));
#8396=CARTESIAN_POINT('Ctrl Pts',(1.02602213787626,-0.492338924724964,5.03437880857729));
#8397=CARTESIAN_POINT('Ctrl Pts',(1.13166612893175,0.128989441018504,5.06668052554289));
#8398=CARTESIAN_POINT('Ctrl Pts',(0.89034970584236,0.711757684128376,5.09900838789433));
#8399=CARTESIAN_POINT('Ctrl Pts',(0.375583834764511,1.07707957256597,5.13136022647449));
#8400=CARTESIAN_POINT('Ctrl Pts',(-0.255070373989398,1.1125503833894,5.16373388639704));
#8401=CARTESIAN_POINT('Ctrl Pts',(-0.808266612488616,0.806867014603004,
5.19612713158992));
#8402=CARTESIAN_POINT('Ctrl Pts',(-1.11420070816338,0.253411220794365,5.22853784854267));
#8403=CARTESIAN_POINT('Ctrl Pts',(-1.07877100089406,-0.378265696239001,
5.26096359350033));
#8404=CARTESIAN_POINT('Ctrl Pts',(-0.712560292595334,-0.894509866678123,
5.29340262757595));
#8405=CARTESIAN_POINT('Ctrl Pts',(-0.127650607355885,-1.13681080552691,
5.32585163203065));
#8406=CARTESIAN_POINT('Ctrl Pts',(0.496644911088633,-1.03091288864219,5.35831080085294));
#8407=CARTESIAN_POINT('Ctrl Pts',(0.968925991004248,-0.608726803401192,
5.39077254625792));
#8408=CARTESIAN_POINT('Ctrl Pts',(1.08573126301311,-0.203385678647448,5.41242485487802));
#8409=CARTESIAN_POINT('Ctrl Pts',(1.08575865405747,8.19725653867553E-5,
5.42324075872855));
#8410=CARTESIAN_POINT('Ctrl Pts',(0.962721347542879,-0.00411661163177441,
2.15234685977571));
#8411=CARTESIAN_POINT('Ctrl Pts',(0.962697036439002,0.17647243326112,2.16194658599263));
#8412=CARTESIAN_POINT('Ctrl Pts',(0.859106513837746,0.53539067596772,2.18112130305809));
#8413=CARTESIAN_POINT('Ctrl Pts',(0.441523188737198,0.908498155871786,2.20981828668204));
#8414=CARTESIAN_POINT('Ctrl Pts',(-0.109164096041492,1.00171508855228,2.23844766404908));
#8415=CARTESIAN_POINT('Ctrl Pts',(-0.623968541999703,0.788299051013983,
2.26701152025929));
#8416=CARTESIAN_POINT('Ctrl Pts',(-0.945582885707644,0.334666298512384,
2.29551065902089));
#8417=CARTESIAN_POINT('Ctrl Pts',(-0.976516553994219,-0.219280947897082,
2.3239465404964));
#8418=CARTESIAN_POINT('Ctrl Pts',(-0.708579872107489,-0.70374057431398,
2.35232039322412));
#8419=CARTESIAN_POINT('Ctrl Pts',(-0.225007223597382,-0.970809187175863,
2.3806336417432));
#8420=CARTESIAN_POINT('Ctrl Pts',(0.325378852667097,-0.93976097174502,2.40888765462467));
#8421=CARTESIAN_POINT('Ctrl Pts',(0.773967917830734,-0.621252530146527,
2.43708398784343));
#8422=CARTESIAN_POINT('Ctrl Pts',(0.983916611731044,-0.114028404154294,
2.46522395532223));
#8423=CARTESIAN_POINT('Ctrl Pts',(0.892012622004092,0.426349139204185,2.49330953081928));
#8424=CARTESIAN_POINT('Ctrl Pts',(0.588120879377049,0.765771851692147,2.51666932886635));
#8425=CARTESIAN_POINT('Ctrl Pts',(0.265171410425461,0.909790782859939,2.53533257394823));
#8426=CARTESIAN_POINT('Ctrl Pts',(0.00295104918847766,0.946918837023357,
2.54931723993354));
#8427=CARTESIAN_POINT('Ctrl Pts',(-0.259128227762097,0.909851006157386,
2.56328950518113));
#8428=CARTESIAN_POINT('Ctrl Pts',(-0.500519402075947,0.801866490451361,
2.57724962652205));
#8429=CARTESIAN_POINT('Ctrl Pts',(-0.702277143832267,0.631373250483782,
2.5911976605843));
#8430=CARTESIAN_POINT('Ctrl Pts',(-0.88723717920968,0.355036238046743,2.60874752373027));
#8431=CARTESIAN_POINT('Ctrl Pts',(-0.952446153747716,0.0325776524498273,
2.62575995705517));
#8432=CARTESIAN_POINT('Ctrl Pts',(-0.897957539757315,-0.274233551693925,
2.64224109774197));
#8433=CARTESIAN_POINT('Ctrl Pts',(-0.770255823431421,-0.558036376433486,
2.65871051814366));
#8434=CARTESIAN_POINT('Ctrl Pts',(-0.485357076941816,-0.836110903690922,
2.67927513518536));
#8435=CARTESIAN_POINT('Ctrl Pts',(-0.0775319663989175,-0.950476259880596,
2.7011828579738));
#8436=CARTESIAN_POINT('Ctrl Pts',(0.386529697138345,-0.884891476815102,
2.7258038844267));
#8437=CARTESIAN_POINT('Ctrl Pts',(0.777236927466001,-0.595055584395186,
2.75039346878802));
#8438=CARTESIAN_POINT('Ctrl Pts',(0.956995355922048,-0.097529407098393,
2.77767868535629));
#8439=CARTESIAN_POINT('Ctrl Pts',(0.886438324246732,0.371210169594461,2.80220878560151));
#8440=CARTESIAN_POINT('Ctrl Pts',(0.599889044325121,0.749619302024166,2.8267136473443));
#8441=CARTESIAN_POINT('Ctrl Pts',(0.216229858198713,0.92235427561694,2.84847500153269));
#8442=CARTESIAN_POINT('Ctrl Pts',(-0.249196296007761,0.926605057610193,
2.87293857301302));
#8443=CARTESIAN_POINT('Ctrl Pts',(-0.748339976156685,0.662149208528223,
2.90145349416336));
#8444=CARTESIAN_POINT('Ctrl Pts',(-1.00784252719217,0.00108226136453731,
2.93671648399365));
#8445=CARTESIAN_POINT('Ctrl Pts',(-0.738609749853676,-0.683953218299274,
2.97329856217955));
#8446=CARTESIAN_POINT('Ctrl Pts',(-0.0760369512723759,-1.0030387720919,
3.00984720605691));
#8447=CARTESIAN_POINT('Ctrl Pts',(0.626253849277891,-0.78633880600751,3.04636816423152));
#8448=CARTESIAN_POINT('Ctrl Pts',(0.993305041368912,-0.150207345540429,
3.08286657411111));
#8449=CARTESIAN_POINT('Ctrl Pts',(0.830107070720763,0.565297577569166,3.1193475619553));
#8450=CARTESIAN_POINT('Ctrl Pts',(0.223310847090626,0.979012770835039,3.15581708462796));
#8451=CARTESIAN_POINT('Ctrl Pts',(-0.420703939193676,0.880994726407311,
3.18822751837814));
#8452=CARTESIAN_POINT('Ctrl Pts',(-0.813020823197554,0.496480837443196,
3.21658791513038));
#8453=CARTESIAN_POINT('Ctrl Pts',(-0.95195527204512,0.0475836205868763,
3.24089647232581));
#8454=CARTESIAN_POINT('Ctrl Pts',(-0.858475820711094,-0.413990349512743,
3.26521013485892));
#8455=CARTESIAN_POINT('Ctrl Pts',(-0.58969183309083,-0.733533759079077,
3.28682351737405));
#8456=CARTESIAN_POINT('Ctrl Pts',(-0.174261433996607,-0.938557040943953,
3.31114684834291));
#8457=CARTESIAN_POINT('Ctrl Pts',(0.252658678818904,-0.92116569916459,3.33277106740655));
#8458=CARTESIAN_POINT('Ctrl Pts',(0.694802991231644,-0.656123967968513,
3.35981348087761));
#8459=CARTESIAN_POINT('Ctrl Pts',(0.939291519468958,-0.241256077865081,
3.38416158448978));
#8460=CARTESIAN_POINT('Ctrl Pts',(0.91218681845093,0.282668180662149,3.41123151679007));
#8461=CARTESIAN_POINT('Ctrl Pts',(0.666683572839207,0.68499526322474,3.43560763134909));
#8462=CARTESIAN_POINT('Ctrl Pts',(0.257903664472838,0.920757528699098,3.45999919062152));
#8463=CARTESIAN_POINT('Ctrl Pts',(-0.293190683850414,0.935856697443789,
3.48847629875965));
#8464=CARTESIAN_POINT('Ctrl Pts',(-0.835253605337006,0.567793133594608,
3.52105113144131));
#8465=CARTESIAN_POINT('Ctrl Pts',(-0.971269459465228,-0.0320272028560387,
3.5516285035243));
#8466=CARTESIAN_POINT('Ctrl Pts',(-0.815479303068769,-0.473036420310123,
3.57611817473918));
#8467=CARTESIAN_POINT('Ctrl Pts',(-0.587134159411761,-0.73912653502778,
3.59449938665691));
#8468=CARTESIAN_POINT('Ctrl Pts',(-0.276488049756515,-0.903067474146875,
3.61289387563012));
#8469=CARTESIAN_POINT('Ctrl Pts',(0.111480528612638,-0.94714988836231,3.63334893620245));
#8470=CARTESIAN_POINT('Ctrl Pts',(0.524623823248839,-0.808457946093702,
3.65587122236952));
#8471=CARTESIAN_POINT('Ctrl Pts',(0.848331491884379,-0.459374496378889,
3.68047110361084));
#8472=CARTESIAN_POINT('Ctrl Pts',(0.937726582189932,-0.108362961515514,
3.699198284524));
#8473=CARTESIAN_POINT('Ctrl Pts',(0.920661842541678,0.132470309013187,3.71203717388858));
#8474=CARTESIAN_POINT('Ctrl Pts',(0.884364839801641,0.30246672743071,3.7212845535523));
#8475=CARTESIAN_POINT('Ctrl Pts',(0.759456347652235,0.582682043325935,3.73747601951444));
#8476=CARTESIAN_POINT('Ctrl Pts',(0.422964808729093,0.883858075393611,3.76063152662413));
#8477=CARTESIAN_POINT('Ctrl Pts',(-0.112512540933623,0.974918894479097,
3.78846289755193));
#8478=CARTESIAN_POINT('Ctrl Pts',(-0.614996115744401,0.766897370709679,
3.81633979986252));
#8479=CARTESIAN_POINT('Ctrl Pts',(-0.930417714207424,0.322614824716656,
3.84426444412183));
#8480=CARTESIAN_POINT('Ctrl Pts',(-0.961140988257394,-0.222324918431914,
3.87223838421193));
#8481=CARTESIAN_POINT('Ctrl Pts',(-0.69677120594697,-0.700969958174984,
3.9002634148559));
#8482=CARTESIAN_POINT('Ctrl Pts',(-0.217362760794632,-0.96609476978467,
3.92834117714213));
#8483=CARTESIAN_POINT('Ctrl Pts',(0.330671812874561,-0.935470664097115,
3.95647331440789));
#8484=CARTESIAN_POINT('Ctrl Pts',(0.779309073310336,-0.617338693461153,
3.98466140544244));
#8485=CARTESIAN_POINT('Ctrl Pts',(0.990347687928942,-0.108251830746577,
4.01290698107989));
#8486=CARTESIAN_POINT('Ctrl Pts',(0.898013637895048,0.436226331588933,4.04121153220018));
#8487=CARTESIAN_POINT('Ctrl Pts',(0.529328619401076,0.84897754575353,4.06957647148122));
#8488=CARTESIAN_POINT('Ctrl Pts',(-0.00352717617365774,1.00269376187457,
4.09800320508173));
#8489=CARTESIAN_POINT('Ctrl Pts',(-0.53787017868102,0.848886205494921,4.12649296047967));
#8490=CARTESIAN_POINT('Ctrl Pts',(-0.895195474546552,0.44904748125299,4.15398961563631));
#8491=CARTESIAN_POINT('Ctrl Pts',(-0.99698925472466,-0.0540344302060386,
4.18048581348479));
#8492=CARTESIAN_POINT('Ctrl Pts',(-0.851356000818643,-0.524614091200913,
4.20597562966137));
#8493=CARTESIAN_POINT('Ctrl Pts',(-0.439393797688116,-0.929156781447132,
4.23577571608365));
#8494=CARTESIAN_POINT('Ctrl Pts',(0.239134479307232,-1.03172425268404,4.26992283604039));
#8495=CARTESIAN_POINT('Ctrl Pts',(0.88062635002243,-0.595308924912992,4.30846235818722));
#8496=CARTESIAN_POINT('Ctrl Pts',(1.05387305271645,0.162865133152882,4.34712801875718));
#8497=CARTESIAN_POINT('Ctrl Pts',(0.664364503263854,0.839011374927392,4.38592206739164));
#8498=CARTESIAN_POINT('Ctrl Pts',(-0.0845907046652596,1.07052624790495,
4.42484600837287));
#8499=CARTESIAN_POINT('Ctrl Pts',(-0.712842695379716,0.767247970283082,
4.45956176146268));
#8500=CARTESIAN_POINT('Ctrl Pts',(-0.994185348275163,0.248487058242295,
4.49002428484184));
#8501=CARTESIAN_POINT('Ctrl Pts',(-0.994274270717777,-0.257467969569223,
4.51619461558179));
#8502=CARTESIAN_POINT('Ctrl Pts',(-0.751855150970942,-0.70361733908245,
4.54242443744114));
#8503=CARTESIAN_POINT('Ctrl Pts',(-0.324470129231318,-0.979336141683844,
4.56871404297466));
#8504=CARTESIAN_POINT('Ctrl Pts',(0.183878891843407,-1.0179645870293,4.59506396293236));
#8505=CARTESIAN_POINT('Ctrl Pts',(0.581751730736977,-0.838265598761856,
4.61762222395677));
#8506=CARTESIAN_POINT('Ctrl Pts',(0.825328076283757,-0.580104449599382,
4.63636280804653));
#8507=CARTESIAN_POINT('Ctrl Pts',(0.998586089801493,-0.245951087937804,
4.65623122227954));
#8508=CARTESIAN_POINT('Ctrl Pts',(1.02625485131006,0.238581037359652,4.68111440254546));
#8509=CARTESIAN_POINT('Ctrl Pts',(0.743789931407803,0.74997765265919,4.7110508969794));
#8510=CARTESIAN_POINT('Ctrl Pts',(0.231451184999164,1.03337076367631,4.74106392441336));
#8511=CARTESIAN_POINT('Ctrl Pts',(-0.354721818349007,1.0006818484025,4.7711534400235));
#8512=CARTESIAN_POINT('Ctrl Pts',(-0.834827143804072,0.660265838075267,
4.80131925998906));
#8513=CARTESIAN_POINT('Ctrl Pts',(-1.06081927769198,0.115228410684275,4.83156116578106));
#8514=CARTESIAN_POINT('Ctrl Pts',(-0.961937848645582,-0.467962848556256,
4.86187885676498));
#8515=CARTESIAN_POINT('Ctrl Pts',(-0.566959468281633,-0.910252364800106,
4.89227197078685));
#8516=CARTESIAN_POINT('Ctrl Pts',(0.00419774968818196,-1.07501280772215,
4.92274007833275));
#8517=CARTESIAN_POINT('Ctrl Pts',(0.576862797925814,-0.910241916881616,
4.95328268065342));
#8518=CARTESIAN_POINT('Ctrl Pts',(0.975048407214078,-0.464974479905994,
4.98389921569725));
#8519=CARTESIAN_POINT('Ctrl Pts',(1.07554249229,0.125301228542384,5.01458905199364));
#8520=CARTESIAN_POINT('Ctrl Pts',(0.846043667387722,0.679874836165035,5.04535150127358));
#8521=CARTESIAN_POINT('Ctrl Pts',(0.355525902562435,1.02815400916832,5.07618579327906));
#8522=CARTESIAN_POINT('Ctrl Pts',(-0.246487037256726,1.06215264226365,5.10709113070068));
#8523=CARTESIAN_POINT('Ctrl Pts',(-0.775512215175448,0.769987306507226,
5.13806658010937));
#8524=CARTESIAN_POINT('Ctrl Pts',(-1.06866263704341,0.239955456649329,5.16911131550179));
#8525=CARTESIAN_POINT('Ctrl Pts',(-1.03481521163521,-0.366119450751765,
5.20022407990668));
#8526=CARTESIAN_POINT('Ctrl Pts',(-0.682953505990723,-0.862389869623227,
5.23140440347673));
#8527=CARTESIAN_POINT('Ctrl Pts',(-0.119822206743421,-1.09583181987539,
5.26264991422472));
#8528=CARTESIAN_POINT('Ctrl Pts',(0.482414728890113,-0.99383199184833,5.29396235184144));
#8529=CARTESIAN_POINT('Ctrl Pts',(0.938933400305489,-0.585955811533194,
5.32533420344708));
#8530=CARTESIAN_POINT('Ctrl Pts',(1.05214732608714,-0.193544083814575,5.34629921120176));
#8531=CARTESIAN_POINT('Ctrl Pts',(1.05217386845809,0.00361940518297847,
5.35677999931289));
#8532=CARTESIAN_POINT('Ctrl Pts',(1.03720012607221,-0.00409632044393359,
2.15215376000718));
#8533=CARTESIAN_POINT('Ctrl Pts',(1.0371739562621,0.190299665690889,2.1624874336011));
#8534=CARTESIAN_POINT('Ctrl Pts',(0.92558272158616,0.577069833109404,2.18315020057125));
#8535=CARTESIAN_POINT('Ctrl Pts',(0.475702554611024,0.978996718760897,2.21406476939329));
#8536=CARTESIAN_POINT('Ctrl Pts',(-0.117602071922459,1.0794537551305,2.24491151338212));
#8537=CARTESIAN_POINT('Ctrl Pts',(-0.67223251082179,0.849511405004554,2.27568514165904));
#8538=CARTESIAN_POINT('Ctrl Pts',(-1.01868605409155,0.360824868161801,2.30638700631186));
#8539=CARTESIAN_POINT('Ctrl Pts',(-1.05198527374106,-0.235832800197401,
2.33701552683969));
#8540=CARTESIAN_POINT('Ctrl Pts',(-0.763435051280867,-0.757511025548864,
2.36757050042531));
#8541=CARTESIAN_POINT('Ctrl Pts',(-0.242837916088414,-1.0449929062352,2.39805118245125));
#8542=CARTESIAN_POINT('Ctrl Pts',(0.349453096149757,-1.01154391433838,2.42845715295811));
#8543=CARTESIAN_POINT('Ctrl Pts',(0.83196489491292,-0.668897917475794,2.45878794166022));
#8544=CARTESIAN_POINT('Ctrl Pts',(1.05764301678683,-0.123543606707892,2.48904318489043));
#8545=CARTESIAN_POINT('Ctrl Pts',(0.958836971515402,0.457095916413721,2.51922258240279));
#8546=CARTESIAN_POINT('Ctrl Pts',(0.632465576049352,0.821551271589622,2.54430864803126));
#8547=CARTESIAN_POINT('Ctrl Pts',(0.285855566773319,0.976108708850338,2.56433940263466));
#8548=CARTESIAN_POINT('Ctrl Pts',(0.00452756006785972,1.01593379748638,
2.57934338276949));
#8549=CARTESIAN_POINT('Ctrl Pts',(-0.2765370042666,0.976170788344264,2.59432827452502));
#8550=CARTESIAN_POINT('Ctrl Pts',(-0.535307761035302,0.86040144442448,2.60929405779257));
#8551=CARTESIAN_POINT('Ctrl Pts',(-0.751497261576938,0.677699097345559,
2.62424075774338));
#8552=CARTESIAN_POINT('Ctrl Pts',(-0.949595343425886,0.381711610440999,
2.64303841886695));
#8553=CARTESIAN_POINT('Ctrl Pts',(-1.01936200319434,0.0365227623030728,
2.66125102072396));
#8554=CARTESIAN_POINT('Ctrl Pts',(-0.961064851420158,-0.291671978015799,
2.67888133848244));
#8555=CARTESIAN_POINT('Ctrl Pts',(-0.824511437821258,-0.595122439806544,
2.6964916259616));
#8556=CARTESIAN_POINT('Ctrl Pts',(-0.520048507305593,-0.892224089661673,
2.71846705734819));
#8557=CARTESIAN_POINT('Ctrl Pts',(-0.0846891312651837,-1.01424813098015,
2.74185404671718));
#8558=CARTESIAN_POINT('Ctrl Pts',(0.410258207256074,-0.944271157163008,
2.76811431360273));
#8559=CARTESIAN_POINT('Ctrl Pts',(0.826474742453967,-0.635355915055917,
2.79431536270512));
#8560=CARTESIAN_POINT('Ctrl Pts',(1.0176655081718,-0.105925126889566,2.82335070844217));
#8561=CARTESIAN_POINT('Ctrl Pts',(0.942602044217525,0.392253570097308,2.8494235300747));
#8562=CARTESIAN_POINT('Ctrl Pts',(0.638357555434203,0.793903498901933,2.87543765808239));
#8563=CARTESIAN_POINT('Ctrl Pts',(0.231584750247889,0.976964213416025,2.89850945113229));
#8564=CARTESIAN_POINT('Ctrl Pts',(-0.261300417458962,0.981432732038026,
2.92441673147305));
#8565=CARTESIAN_POINT('Ctrl Pts',(-0.78911757047424,0.701577318097918,2.95457534274698));
#8566=CARTESIAN_POINT('Ctrl Pts',(-1.06274273585526,0.00369915306037486,
2.99179914126635));
#8567=CARTESIAN_POINT('Ctrl Pts',(-0.778888284969809,-0.717626824525481,
3.03032832205921));
#8568=CARTESIAN_POINT('Ctrl Pts',(-0.0825571702149149,-1.05259129336624,
3.06873400475036));
#8569=CARTESIAN_POINT('Ctrl Pts',(0.653482636017743,-0.82510163125457,3.10701834952163));
#8570=CARTESIAN_POINT('Ctrl Pts',(1.03694987840345,-0.159780933193991,3.14518392884017));
#8571=CARTESIAN_POINT('Ctrl Pts',(0.866376317169457,0.586342300918658,3.1832336854523));
#8572=CARTESIAN_POINT('Ctrl Pts',(0.234998019991916,1.01633566146955,3.22117007239323));
#8573=CARTESIAN_POINT('Ctrl Pts',(-0.432991952034301,0.914309265779491,
3.25479444760821));
#8574=CARTESIAN_POINT('Ctrl Pts',(-0.838878119080994,0.516296390053429,
3.2841451151001));
#8575=CARTESIAN_POINT('Ctrl Pts',(-0.982273687442794,0.0525680030763169,
3.30925761409405));
#8576=CARTESIAN_POINT('Ctrl Pts',(-0.885793450990451,-0.423240964042453,
3.33432279750852));
#8577=CARTESIAN_POINT('Ctrl Pts',(-0.609137316783548,-0.751973908577496,
3.35656577614145));
#8578=CARTESIAN_POINT('Ctrl Pts',(-0.182387946913773,-0.962521184839306,
3.38155029819673));
#8579=CARTESIAN_POINT('Ctrl Pts',(0.255309527200463,-0.944507833568579,
3.40372342590835));
#8580=CARTESIAN_POINT('Ctrl Pts',(0.707637937756388,-0.673273572524831,
3.43139261558955));
#8581=CARTESIAN_POINT('Ctrl Pts',(0.95709097082737,-0.249569786756698,3.45625502960754));
#8582=CARTESIAN_POINT('Ctrl Pts',(0.929340031620981,0.2840721590868,3.48382950356397));
#8583=CARTESIAN_POINT('Ctrl Pts',(0.679684036454164,0.692970704905364,3.50860996446133));
#8584=CARTESIAN_POINT('Ctrl Pts',(0.264972950420313,0.932018810712846,3.53335442277599));
#8585=CARTESIAN_POINT('Ctrl Pts',(-0.292875541075979,0.947146888293306,
3.56218205848296));
#8586=CARTESIAN_POINT('Ctrl Pts',(-0.83992957344522,0.575232532689319,3.59507362871049));
#8587=CARTESIAN_POINT('Ctrl Pts',(-0.976446149645535,-0.0285021060551591,
3.62585138286231));
#8588=CARTESIAN_POINT('Ctrl Pts',(-0.819982137782929,-0.471194465906437,
3.65043867935641));
#8589=CARTESIAN_POINT('Ctrl Pts',(-0.591068510913671,-0.737865206766389,
3.66886289728087));
#8590=CARTESIAN_POINT('Ctrl Pts',(-0.28016561471819,-0.901875466186263,
3.68727288345947));
#8591=CARTESIAN_POINT('Ctrl Pts',(0.107481257946226,-0.945857362484449,
3.70771184020532));
#8592=CARTESIAN_POINT('Ctrl Pts',(0.519462496772379,-0.807428539347808,
3.73017500517365));
#8593=CARTESIAN_POINT('Ctrl Pts',(0.841496073287022,-0.459974006299116,
3.75465525952053));
#8594=CARTESIAN_POINT('Ctrl Pts',(0.93019017290814,-0.111360958781802,3.77325611214999));
#8595=CARTESIAN_POINT('Ctrl Pts',(0.913264927019297,0.127451186282573,3.78598775165775));
#8596=CARTESIAN_POINT('Ctrl Pts',(0.877290869596397,0.295921312263089,3.79515241068551));
#8597=CARTESIAN_POINT('Ctrl Pts',(0.753583159450096,0.573375486738159,3.8111856372686));
#8598=CARTESIAN_POINT('Ctrl Pts',(0.420870761936589,0.870973318960077,3.83407713920392));
#8599=CARTESIAN_POINT('Ctrl Pts',(-0.10719372434703,0.960591213795104,3.86152417393542));
#8600=CARTESIAN_POINT('Ctrl Pts',(-0.601464341491623,0.755785630251061,
3.88895202302946));
#8601=CARTESIAN_POINT('Ctrl Pts',(-0.910906330100926,0.319626006652346,
3.91636240063127));
#8602=CARTESIAN_POINT('Ctrl Pts',(-0.940819883683162,-0.214000382719056,
3.94375782125121));
#8603=CARTESIAN_POINT('Ctrl Pts',(-0.682385307441754,-0.681546976981073,
3.97114042705916));
#8604=CARTESIAN_POINT('Ctrl Pts',(-0.214987241307903,-0.939836825243413,
3.99851254259768));
#8605=CARTESIAN_POINT('Ctrl Pts',(0.318023095443073,-0.909885582634909,
4.02587641384691));
#8606=CARTESIAN_POINT('Ctrl Pts',(0.7533132090918,-0.601017068726198,4.05323432668543));
#8607=CARTESIAN_POINT('Ctrl Pts',(0.957524926712381,-0.10797780366471,4.0805885629404));
#8608=CARTESIAN_POINT('Ctrl Pts',(0.868146657813169,0.418119687888217,4.1079413947471));
#8609=CARTESIAN_POINT('Ctrl Pts',(0.51252087301969,0.816016703834251,4.13529515584408));
#8610=CARTESIAN_POINT('Ctrl Pts',(-0.000280531296823317,0.96378804214646,
4.16265203940924));
#8611=CARTESIAN_POINT('Ctrl Pts',(-0.513389900953546,0.815932837409874,
4.19001455783718));
#8612=CARTESIAN_POINT('Ctrl Pts',(-0.855769768104171,0.432614499437845,
4.21637087266359));
#8613=CARTESIAN_POINT('Ctrl Pts',(-0.953045996844169,-0.0487133751138879,
4.2417227597978));
#8614=CARTESIAN_POINT('Ctrl Pts',(-0.813879110112111,-0.498125538648156,
4.26606827749635));
#8615=CARTESIAN_POINT('Ctrl Pts',(-0.420960341352675,-0.883784830320034,
4.29448506591828));
#8616=CARTESIAN_POINT('Ctrl Pts',(0.224789069817019,-0.981132664539065,
4.32698303203636));
#8617=CARTESIAN_POINT('Ctrl Pts',(0.833681922437495,-0.56650552027897,4.36357743712977));
#8618=CARTESIAN_POINT('Ctrl Pts',(0.997525969733803,0.151809280111847,4.40021093558096));
#8619=CARTESIAN_POINT('Ctrl Pts',(0.629053416259707,0.790872367938504,4.43688813066444));
#8620=CARTESIAN_POINT('Ctrl Pts',(-0.0776376842752591,1.00903081883449,
4.47361454615104));
#8621=CARTESIAN_POINT('Ctrl Pts',(-0.669159294915032,0.723239602156119,
4.50630883475876));
#8622=CARTESIAN_POINT('Ctrl Pts',(-0.933615302724183,0.235422240437012,
4.53495405715562));
#8623=CARTESIAN_POINT('Ctrl Pts',(-0.933641466162531,-0.239764602920034,
4.55953364433428));
#8624=CARTESIAN_POINT('Ctrl Pts',(-0.706144252215777,-0.65830114813711,
4.58414298960005));
#8625=CARTESIAN_POINT('Ctrl Pts',(-0.305568054713619,-0.916660441466946,
4.60878302433065));
#8626=CARTESIAN_POINT('Ctrl Pts',(0.170387676510673,-0.952765931836802,
4.63345394982545));
#8627=CARTESIAN_POINT('Ctrl Pts',(0.542555110244804,-0.784634851727257,
4.65455753095455));
#8628=CARTESIAN_POINT('Ctrl Pts',(0.770225790729519,-0.54331566877176,4.67207538305286));
#8629=CARTESIAN_POINT('Ctrl Pts',(0.932090725649148,-0.231113115898143,
4.69063876644602));
#8630=CARTESIAN_POINT('Ctrl Pts',(0.957871337899541,0.221285409072723,4.71387291471119));
#8631=CARTESIAN_POINT('Ctrl Pts',(0.694319442459975,0.698311633436892,4.74180038845792));
#8632=CARTESIAN_POINT('Ctrl Pts',(0.216737061340996,0.962418705490843,4.76977721937668));
#8633=CARTESIAN_POINT('Ctrl Pts',(-0.329241357561265,0.931920409055914,
4.79780471923481));
#8634=CARTESIAN_POINT('Ctrl Pts',(-0.776106758281407,0.615017342938231,
4.82588478924082));
#8635=CARTESIAN_POINT('Ctrl Pts',(-0.986303575858324,0.107968492198592,
4.85401898069626));
#8636=CARTESIAN_POINT('Ctrl Pts',(-0.894329856751629,-0.434269986929119,
4.8822089287795));
#8637=CARTESIAN_POINT('Ctrl Pts',(-0.527226968394228,-0.845299850272977,
4.91045615450255));
#8638=CARTESIAN_POINT('Ctrl Pts',(0.0033919611434381,-0.998340479227608,
4.93876214814565));
#8639=CARTESIAN_POINT('Ctrl Pts',(0.535231960194268,-0.845295789931832,
4.96712834313108));
#8640=CARTESIAN_POINT('Ctrl Pts',(0.904933168151654,-0.431859589715681,
4.9955561182682));
#8641=CARTESIAN_POINT('Ctrl Pts',(0.998215666603856,0.116109753255343,5.02404679691162));
#8642=CARTESIAN_POINT('Ctrl Pts',(0.785186438599943,0.630876060238445,5.0526016457263));
#8643=CARTESIAN_POINT('Ctrl Pts',(0.329897474700307,0.954144141946419,5.0812218763083));
#8644=CARTESIAN_POINT('Ctrl Pts',(-0.22889329357451,0.985708576145502,5.10990864545268));
#8645=CARTESIAN_POINT('Ctrl Pts',(-0.719987155661827,0.714505791718518,
5.13866303733357));
#8646=CARTESIAN_POINT('Ctrl Pts',(-0.992173120872884,0.222413780858762,
5.16748611276041));
#8647=CARTESIAN_POINT('Ctrl Pts',(-0.960763757484564,-0.340411422023257,
5.19637880363374));
#8648=CARTESIAN_POINT('Ctrl Pts',(-0.633940084188984,-0.80142093923978,
5.22534214530267));
#8649=CARTESIAN_POINT('Ctrl Pts',(-0.110673692443478,-1.01836625645358,
5.25437676792106));
#8650=CARTESIAN_POINT('Ctrl Pts',(0.449182451185127,-0.923606231726753,
5.28348405622099));
#8651=CARTESIAN_POINT('Ctrl Pts',(0.873798643905496,-0.544251784946238,
5.31266356415371));
#8652=CARTESIAN_POINT('Ctrl Pts',(0.979170353153057,-0.17920951900525,5.33216668867801));
#8653=CARTESIAN_POINT('Ctrl Pts',(0.979195073394965,0.00441873155204175,
5.34192797255006));
#8654=CARTESIAN_POINT('Ctrl Pts',(1.08383455515366,-0.00100513229999224,
2.09412075287127));
#8655=CARTESIAN_POINT('Ctrl Pts',(1.0838072186452,0.202057385077309,2.10491512067412));
#8656=CARTESIAN_POINT('Ctrl Pts',(0.967176636812093,0.606569610116454,2.12652636292198));
#8657=CARTESIAN_POINT('Ctrl Pts',(0.496066254774699,1.02763200736581,2.15890649001074));
#8658=CARTESIAN_POINT('Ctrl Pts',(-0.126357494462602,1.13317581705174,2.19127042803801));
#8659=CARTESIAN_POINT('Ctrl Pts',(-0.709205564145551,0.891686385254436,
2.22360804916189));
#8660=CARTESIAN_POINT('Ctrl Pts',(-1.0739333900271,0.377472593954113,2.25592086261441));
#8661=CARTESIAN_POINT('Ctrl Pts',(-1.10916844440495,-0.251400260581686,
2.28820514288567));
#8662=CARTESIAN_POINT('Ctrl Pts',(-0.804703166881614,-0.802127600795733,
2.32045953364164));
#8663=CARTESIAN_POINT('Ctrl Pts',(-0.254453640242555,-1.10613142625631,
2.35268161694683));
#8664=CARTESIAN_POINT('Ctrl Pts',(0.372524133280107,-1.07084797948588,2.38486953313084));
#8665=CARTESIAN_POINT('Ctrl Pts',(0.884048629344189,-0.707746783112836,
2.4170211098838));
#8666=CARTESIAN_POINT('Ctrl Pts',(1.12368139865338,-0.128967810912809,2.44913462963003));
#8667=CARTESIAN_POINT('Ctrl Pts',(1.01879159895331,0.488100661391317,2.48120765737687));
#8668=CARTESIAN_POINT('Ctrl Pts',(0.671592645081585,0.875945276774875,2.50790086584788));
#8669=CARTESIAN_POINT('Ctrl Pts',(0.30248923948297,1.04055255032915,2.52923217303823));
#8670=CARTESIAN_POINT('Ctrl Pts',(0.00273063932233121,1.08299928584134,
2.54521959464766));
#8671=CARTESIAN_POINT('Ctrl Pts',(-0.296918707076225,1.04061966320984,2.56119554297854));
#8672=CARTESIAN_POINT('Ctrl Pts',(-0.57295347024857,0.917140579769783,2.57715977596269));
#8673=CARTESIAN_POINT('Ctrl Pts',(-0.803692754746948,0.722157016036992,
2.59311219792725));
#8674=CARTESIAN_POINT('Ctrl Pts',(-1.0152363324343,0.406108796017378,2.61318476146475));
#8675=CARTESIAN_POINT('Ctrl Pts',(-1.08983178300628,0.037250869792953,2.63264744709217));
#8676=CARTESIAN_POINT('Ctrl Pts',(-1.02750791393542,-0.31367372199185,2.65149873120761));
#8677=CARTESIAN_POINT('Ctrl Pts',(-0.881447705942929,-0.638275149283354,
2.67033658335757));
#8678=CARTESIAN_POINT('Ctrl Pts',(-0.555598070387777,-0.956318325625562,
2.69385882342524));
#8679=CARTESIAN_POINT('Ctrl Pts',(-0.0892637312173702,-1.08706975249208,
2.71891053244989));
#8680=CARTESIAN_POINT('Ctrl Pts',(0.441231110674361,-1.0120947255311,2.74705695241423));
#8681=CARTESIAN_POINT('Ctrl Pts',(0.887695511526617,-0.680828785898897,
2.77515950943379));
#8682=CARTESIAN_POINT('Ctrl Pts',(1.09296623655105,-0.112574626725122,2.80632510595015));
#8683=CARTESIAN_POINT('Ctrl Pts',(1.01238753003802,0.422468371144573,2.83432700014897));
#8684=CARTESIAN_POINT('Ctrl Pts',(0.685489237407475,0.854090959271124,2.86228097985869));
#8685=CARTESIAN_POINT('Ctrl Pts',(0.24818119515735,1.0509253589982,2.88708521506922));
#8686=CARTESIAN_POINT('Ctrl Pts',(-0.281912505533628,1.05574552847318,2.91494833111401));
#8687=CARTESIAN_POINT('Ctrl Pts',(-0.849831183761748,0.754692758675727,
2.94739661399269));
#8688=CARTESIAN_POINT('Ctrl Pts',(-1.14444668157779,0.00348830941917116,
2.98746544745627));
#8689=CARTESIAN_POINT('Ctrl Pts',(-0.838821075659442,-0.773323040553238,
3.02895622562989));
#8690=CARTESIAN_POINT('Ctrl Pts',(-0.0887510849550236,-1.13418240132233,
3.0703256506113));
#8691=CARTESIAN_POINT('Ctrl Pts',(0.704252876635555,-0.88910978446688,3.11157120272713));
#8692=CARTESIAN_POINT('Ctrl Pts',(1.11741889612126,-0.172268714907602,3.15269084027887));
#8693=CARTESIAN_POINT('Ctrl Pts',(0.933635635982071,0.631579498941108,3.19368244226885));
#8694=CARTESIAN_POINT('Ctrl Pts',(0.253516921328693,1.09472482298316,3.23454449498551));
#8695=CARTESIAN_POINT('Ctrl Pts',(-0.46578270941342,0.984823889831234,3.27074921367188));
#8696=CARTESIAN_POINT('Ctrl Pts',(-0.902683215290603,0.556363270548466,
3.30234310258505));
#8697=CARTESIAN_POINT('Ctrl Pts',(-1.05697667075416,0.05735687056592,3.32936366304358));
#8698=CARTESIAN_POINT('Ctrl Pts',(-0.953160259240073,-0.454456668822736,
3.35632572854271));
#8699=CARTESIAN_POINT('Ctrl Pts',(-0.655710111295285,-0.807878038485106,
3.38023751987761));
#8700=CARTESIAN_POINT('Ctrl Pts',(-0.197041480200333,-1.03414796641898,
3.40708995144052));
#8701=CARTESIAN_POINT('Ctrl Pts',(0.273086892424193,-1.01475766405274,3.43090374642035));
#8702=CARTESIAN_POINT('Ctrl Pts',(0.758645088847692,-0.723565062091646,
3.46060506771804));
#8703=CARTESIAN_POINT('Ctrl Pts',(1.02619655264658,-0.268984419353583,3.4872756034617));
#8704=CARTESIAN_POINT('Ctrl Pts',(0.996387322687455,0.303025364684566,3.51683147442567));
#8705=CARTESIAN_POINT('Ctrl Pts',(0.728951561944792,0.740953674049451,3.54337068720782));
#8706=CARTESIAN_POINT('Ctrl Pts',(0.285110217835692,0.996730445071976,3.56984942607481));
#8707=CARTESIAN_POINT('Ctrl Pts',(-0.311384544736447,1.01283968272107,3.60067110558919));
#8708=CARTESIAN_POINT('Ctrl Pts',(-0.895518055039455,0.615482305648,3.6357943259958));
#8709=CARTESIAN_POINT('Ctrl Pts',(-1.0409159420416,-0.0283394110497346,
3.66860908547933));
#8710=CARTESIAN_POINT('Ctrl Pts',(-0.874227166910078,-0.499830766853547,
3.6947954969822));
#8711=CARTESIAN_POINT('Ctrl Pts',(-0.630592962401571,-0.783616493190624,
3.71440219407833));
#8712=CARTESIAN_POINT('Ctrl Pts',(-0.300015163190702,-0.957974480984689,
3.73397463201407));
#8713=CARTESIAN_POINT('Ctrl Pts',(0.111783740171799,-1.00466671708127,3.75568519526895));
#8714=CARTESIAN_POINT('Ctrl Pts',(0.548934143160709,-0.857711337819638,
3.77951940523228));
#8715=CARTESIAN_POINT('Ctrl Pts',(0.890168052144742,-0.489407069594645,
3.8054635732035));
#8716=CARTESIAN_POINT('Ctrl Pts',(0.983967638561348,-0.120456653152492,
3.82514559136655));
#8717=CARTESIAN_POINT('Ctrl Pts',(0.966063153040552,0.132090193079272,3.83860912181926));
#8718=CARTESIAN_POINT('Ctrl Pts',(0.928032981075702,0.310180874839214,3.84829683488476));
#8719=CARTESIAN_POINT('Ctrl Pts',(0.79732422491957,0.603293178112202,3.86523401611496));
#8720=CARTESIAN_POINT('Ctrl Pts',(0.446210687994022,0.917210804455452,3.88938327655937));
#8721=CARTESIAN_POINT('Ctrl Pts',(-0.110068761338206,1.01148074075704,3.91829259262403));
#8722=CARTESIAN_POINT('Ctrl Pts',(-0.629778714922221,0.795980055673373,
3.9471315659034));
#8723=CARTESIAN_POINT('Ctrl Pts',(-0.954492360839048,0.338049134353879,
3.9759016731882));
#8724=CARTESIAN_POINT('Ctrl Pts',(-0.985690335581518,-0.221102775015846,
4.00460364145414));
#8725=CARTESIAN_POINT('Ctrl Pts',(-0.71527423954657,-0.710019115305869,
4.0332386406658));
#8726=CARTESIAN_POINT('Ctrl Pts',(-0.22730521254799,-0.979503584524682,
4.0618077501134));
#8727=CARTESIAN_POINT('Ctrl Pts',(0.327979039642183,-0.948145702873503,
4.09031217793584));
#8728=CARTESIAN_POINT('Ctrl Pts',(0.780465135736674,-0.626881939976658,
4.1187531685785));
#8729=CARTESIAN_POINT('Ctrl Pts',(0.992203650298369,-0.115250509294351,
4.14713201945934));
#8730=CARTESIAN_POINT('Ctrl Pts',(0.899499190924821,0.429452598894815,4.17545011398173));
#8731=CARTESIAN_POINT('Ctrl Pts',(0.531938608728281,0.840456211956105,4.20370881077333));
#8732=CARTESIAN_POINT('Ctrl Pts',(0.00320558862913967,0.992645561888121,
4.23190968257249));
#8733=CARTESIAN_POINT('Ctrl Pts',(-0.524589061186669,0.840384906564921,
4.26005395738908));
#8734=CARTESIAN_POINT('Ctrl Pts',(-0.875886060224354,0.446832139458484,
4.28710339665259));
#8735=CARTESIAN_POINT('Ctrl Pts',(-0.975392699171194,-0.0461734306504795,
4.31306524464901));
#8736=CARTESIAN_POINT('Ctrl Pts',(-0.833014281038782,-0.505523598165439,
4.33795023099546));
#8737=CARTESIAN_POINT('Ctrl Pts',(-0.432085868110668,-0.898848002117052,
4.36693537151759));
#8738=CARTESIAN_POINT('Ctrl Pts',(0.224988129031288,-0.997494004660513,
4.39999650828921));
#8739=CARTESIAN_POINT('Ctrl Pts',(0.842309514128291,-0.576595861558382,
4.43710735610631));
#8740=CARTESIAN_POINT('Ctrl Pts',(1.00752258942579,0.149768590973636,4.47414020946719));
#8741=CARTESIAN_POINT('Ctrl Pts',(0.635768391948925,0.793634591411079,4.51110029373353));
#8742=CARTESIAN_POINT('Ctrl Pts',(-0.0743383737232185,1.01237269509007,
4.54799164202132));
#8743=CARTESIAN_POINT('Ctrl Pts',(-0.666508256149446,0.725845969874338,
4.58072644727242));
#8744=CARTESIAN_POINT('Ctrl Pts',(-0.930500361436642,0.238581639159787,
4.60933197480601));
#8745=CARTESIAN_POINT('Ctrl Pts',(-0.930395932628208,-0.235017133168795,
4.63382810381776));
#8746=CARTESIAN_POINT('Ctrl Pts',(-0.704048414868301,-0.651201238468357,
4.65829980147231));
#8747=CARTESIAN_POINT('Ctrl Pts',(-0.306457717371693,-0.90747432123094,
4.68274942071083));
#8748=CARTESIAN_POINT('Ctrl Pts',(0.164900848925934,-0.943116217052762,
4.70718032224016));
#8749=CARTESIAN_POINT('Ctrl Pts',(0.532586291489543,-0.7768743398517,4.72802875324737));
#8750=CARTESIAN_POINT('Ctrl Pts',(0.757186657608633,-0.538773046044311,
4.7453112080288));
#8751=CARTESIAN_POINT('Ctrl Pts',(0.916668695103853,-0.231094170555637,
4.76360306157553));
#8752=CARTESIAN_POINT('Ctrl Pts',(0.941879012311262,0.213904287027886,4.78645305810177));
#8753=CARTESIAN_POINT('Ctrl Pts',(0.683080673189071,0.681957662619039,4.81385719170469));
#8754=CARTESIAN_POINT('Ctrl Pts',(0.215392937090561,0.940387267485015,4.84124578391745));
#8755=CARTESIAN_POINT('Ctrl Pts',(-0.317945518562309,0.91042074411468,4.86862180210215));
#8756=CARTESIAN_POINT('Ctrl Pts',(-0.753387179512403,0.601407580332747,
4.89598712456847));
#8757=CARTESIAN_POINT('Ctrl Pts',(-0.957643715091763,0.108246828535003,
4.92334415364639));
#8758=CARTESIAN_POINT('Ctrl Pts',(-0.868233611205659,-0.417881537488712,
4.95069508929941));
#8759=CARTESIAN_POINT('Ctrl Pts',(-0.512669209156949,-0.815746003186908,
4.97804224075945));
#8760=CARTESIAN_POINT('Ctrl Pts',(4.31839669338944E-5,-0.963454107947432,
5.00538786962271));
#8761=CARTESIAN_POINT('Ctrl Pts',(0.512769332970879,-0.815744639868486,
5.03273427529492));
#8762=CARTESIAN_POINT('Ctrl Pts',(0.868364986197536,-0.417849081119337,
5.06008373717176));
#8763=CARTESIAN_POINT('Ctrl Pts',(0.957786283176147,0.108348086643308,5.08743854354636));
#8764=CARTESIAN_POINT('Ctrl Pts',(0.753496435761779,0.601605495981712,5.11480096457011));
#8765=CARTESIAN_POINT('Ctrl Pts',(0.317936353225337,0.910686321698448,5.1421732876434));
#8766=CARTESIAN_POINT('Ctrl Pts',(-0.215540765577659,0.940677697820739,
5.16955775201152));
#8767=CARTESIAN_POINT('Ctrl Pts',(-0.683455937250816,0.682116790417354,
5.19695665459153));
#8768=CARTESIAN_POINT('Ctrl Pts',(-0.942253548854584,0.213950549125594,
5.22437212570714));
#8769=CARTESIAN_POINT('Ctrl Pts',(-0.912297345239954,-0.320500930766703,
5.25180662638367));
#8770=CARTESIAN_POINT('Ctrl Pts',(-0.602362624559855,-0.757478419318723,
5.27926181463212));
#8771=CARTESIAN_POINT('Ctrl Pts',(-0.107056118750729,-0.962692795935569,
5.30674105031171));
#8772=CARTESIAN_POINT('Ctrl Pts',(0.421984195787826,-0.873059479070634,
5.33424381353539));
#8773=CARTESIAN_POINT('Ctrl Pts',(0.822562701518577,-0.514974705783212,
5.36177808819317));
#8774=CARTESIAN_POINT('Ctrl Pts',(0.921747231678515,-0.171138641059886,
5.38014514248733));
#8775=CARTESIAN_POINT('Ctrl Pts',(0.921770527134554,0.00190593732143055,
5.38934382105108));
#8776=CARTESIAN_POINT('Ctrl Pts',(1.06702201959591,0.00285043970073984,
2.0215475585234));
#8777=CARTESIAN_POINT('Ctrl Pts',(1.06699508957157,0.202893489956048,2.03218141793157));
#8778=CARTESIAN_POINT('Ctrl Pts',(0.952197003975437,0.601527586454393,2.05347419254553));
#8779=CARTESIAN_POINT('Ctrl Pts',(0.487056211644658,1.01753294235621,2.08545253086904));
#8780=CARTESIAN_POINT('Ctrl Pts',(-0.128863848342645,1.1221315680947,2.11747652423528));
#8781=CARTESIAN_POINT('Ctrl Pts',(-0.706907658382305,0.882825885801358,
2.14954193386969));
#8782=CARTESIAN_POINT('Ctrl Pts',(-1.06947298146975,0.371955511405459,2.18164790285542));
#8783=CARTESIAN_POINT('Ctrl Pts',(-1.10473354554263,-0.254222576858051,
2.21379199658814));
#8784=CARTESIAN_POINT('Ctrl Pts',(-0.801098332840217,-0.803816818903664,
2.24597243091371));
#8785=CARTESIAN_POINT('Ctrl Pts',(-0.251022866900719,-1.107928868166,2.27818709518381));
#8786=CARTESIAN_POINT('Ctrl Pts',(0.377157547542421,-1.07275865606352,2.31043394078));
#8787=CARTESIAN_POINT('Ctrl Pts',(0.890814984617286,-0.708364377644769,
2.34271091875739));
#8788=CARTESIAN_POINT('Ctrl Pts',(1.13206003543397,-0.12616681018466,2.37501578311069));
#8789=CARTESIAN_POINT('Ctrl Pts',(1.02649991184449,0.495927285016085,2.4073466493677));
#8790=CARTESIAN_POINT('Ctrl Pts',(0.675888865904133,0.887802847820554,2.43430832444967));
#8791=CARTESIAN_POINT('Ctrl Pts',(0.302465182735742,1.05436962634722,2.45588912818849));
#8792=CARTESIAN_POINT('Ctrl Pts',(-0.00110925844173351,1.09737681688059,
2.47207972994715));
#8793=CARTESIAN_POINT('Ctrl Pts',(-0.304888662325547,1.05443550943871,2.48827516246545));
#8794=CARTESIAN_POINT('Ctrl Pts',(-0.585016322460578,0.929148428211227,
2.50447514794601));
#8795=CARTESIAN_POINT('Ctrl Pts',(-0.819419308229265,0.731096076322071,
2.52067935421188));
#8796=CARTESIAN_POINT('Ctrl Pts',(-1.03454937622517,0.409738788275447,2.5410898548685));
#8797=CARTESIAN_POINT('Ctrl Pts',(-1.110579327663,0.0341785358218987,2.56090566398939));
#8798=CARTESIAN_POINT('Ctrl Pts',(-1.04705118956169,-0.3236433791638,2.5801267491674));
#8799=CARTESIAN_POINT('Ctrl Pts',(-0.898010236343792,-0.654911589195166,
2.59935087157429));
#8800=CARTESIAN_POINT('Ctrl Pts',(-0.565109570799394,-0.97997251636004,
2.62338602717653));
#8801=CARTESIAN_POINT('Ctrl Pts',(-0.0877645744898903,-1.11391907054818,
2.6490300997342));
#8802=CARTESIAN_POINT('Ctrl Pts',(0.456080346993929,-1.03711194963536,2.67788419010735));
#8803=CARTESIAN_POINT('Ctrl Pts',(0.914673548406407,-0.697098327564633,
2.70674252653505));
#8804=CARTESIAN_POINT('Ctrl Pts',(1.12602774396051,-0.112418131739695,2.73881013194141));
#8805=CARTESIAN_POINT('Ctrl Pts',(1.04307840629854,0.439074671072632,2.76767167730267));
#8806=CARTESIAN_POINT('Ctrl Pts',(0.705668036928256,0.884771411857633,2.79653215624472));
#8807=CARTESIAN_POINT('Ctrl Pts',(0.253455787403711,1.08841958876369,2.82218366694516));
#8808=CARTESIAN_POINT('Ctrl Pts',(-0.295493024176249,1.09346191224925,2.85103797378248));
#8809=CARTESIAN_POINT('Ctrl Pts',(-0.884664851586657,0.781403855485988,
2.88469536651339));
#8810=CARTESIAN_POINT('Ctrl Pts',(-1.19129978902031,0.000581549421014766,
2.92635152585855));
#8811=CARTESIAN_POINT('Ctrl Pts',(-0.873168334733573,-0.809044188315319,
2.96958770031669));
#8812=CARTESIAN_POINT('Ctrl Pts',(-0.08991365677559,-1.18627345200091,3.01279661748751));
#8813=CARTESIAN_POINT('Ctrl Pts',(0.740303848481622,-0.930075865252766,
3.05597296819526));
#8814=CARTESIAN_POINT('Ctrl Pts',(1.17404659392292,-0.178225554833157,3.09911149645123));
#8815=CARTESIAN_POINT('Ctrl Pts',(0.981161351803577,0.666927533936675,3.14220724582939));
#8816=CARTESIAN_POINT('Ctrl Pts',(0.264871552947168,1.15510320472919,3.18525471062778));
#8817=CARTESIAN_POINT('Ctrl Pts',(-0.494428740123167,1.03935387427447,3.2234727638888));
#8818=CARTESIAN_POINT('Ctrl Pts',(-0.956404802565376,0.586449571383587,
3.25687471171129));
#8819=CARTESIAN_POINT('Ctrl Pts',(-1.11979346868318,0.058258331371253,3.28547881446806));
#8820=CARTESIAN_POINT('Ctrl Pts',(-1.00986054768212,-0.484166937058073,
3.31405254369003));
#8821=CARTESIAN_POINT('Ctrl Pts',(-0.694283302029937,-0.859206449360406,
3.33942674184122));
#8822=CARTESIAN_POINT('Ctrl Pts',(-0.20720327925374,-1.09954269454893,3.36794392261175));
#8823=CARTESIAN_POINT('Ctrl Pts',(0.29265908786554,-1.07902180486329,3.39326606792902));
#8824=CARTESIAN_POINT('Ctrl Pts',(0.809475546507311,-0.769138857714769,
3.42487917029462));
#8825=CARTESIAN_POINT('Ctrl Pts',(1.09462539138736,-0.28487361877622,3.45329625277239));
#8826=CARTESIAN_POINT('Ctrl Pts',(1.06291369715779,0.325256037101083,3.48482268248564));
#8827=CARTESIAN_POINT('Ctrl Pts',(0.777434815872461,0.7928386116761,3.5131592168709));
#8828=CARTESIAN_POINT('Ctrl Pts',(0.303177481860876,1.06621189571728,3.54145653166712));
#8829=CARTESIAN_POINT('Ctrl Pts',(-0.334758663253051,1.0835070513843,3.57442250475897));
#8830=CARTESIAN_POINT('Ctrl Pts',(-0.960229074971341,0.658229837595933,
3.61202995640657));
#8831=CARTESIAN_POINT('Ctrl Pts',(-1.11619274136482,-0.0318103647610028,
3.64720653123438));
#8832=CARTESIAN_POINT('Ctrl Pts',(-0.937428906276688,-0.537533778848072,
3.67529509327478));
#8833=CARTESIAN_POINT('Ctrl Pts',(-0.676001017110024,-0.84206151951191,
3.69633537325015));
#8834=CARTESIAN_POINT('Ctrl Pts',(-0.321092341582353,-1.02926596955437,
3.7173506245525));
#8835=CARTESIAN_POINT('Ctrl Pts',(0.121208828079285,-1.07942774678667,3.74067104000155));
#8836=CARTESIAN_POINT('Ctrl Pts',(0.590969798913608,-0.921535378852899,
3.76628537873098));
#8837=CARTESIAN_POINT('Ctrl Pts',(0.957844459619203,-0.525614588470272,
3.79417761398359));
#8838=CARTESIAN_POINT('Ctrl Pts',(1.05876459652488,-0.12875481310516,3.81535214818028));
#8839=CARTESIAN_POINT('Ctrl Pts',(1.0395064635086,0.142927269520196,3.82983622592237));
#8840=CARTESIAN_POINT('Ctrl Pts',(0.998590856068431,0.334531305443016,3.84025938000999));
#8841=CARTESIAN_POINT('Ctrl Pts',(0.857941964811768,0.649944025822184,3.85848631113206));
#8842=CARTESIAN_POINT('Ctrl Pts',(0.479993992774951,0.987881570361023,3.88448594098035));
#8843=CARTESIAN_POINT('Ctrl Pts',(-0.118980327541849,1.08940918853345,3.91561757288294));
#8844=CARTESIAN_POINT('Ctrl Pts',(-0.678729907854082,0.85733025713029,3.94668180840835));
#8845=CARTESIAN_POINT('Ctrl Pts',(-1.02852647823543,0.364047032000577,3.97767703233711));
#8846=CARTESIAN_POINT('Ctrl Pts',(-1.06214407322819,-0.238348644573769,
4.0086026043394));
#8847=CARTESIAN_POINT('Ctrl Pts',(-0.770799167454087,-0.765104131388401,
4.03945751410833));
#8848=CARTESIAN_POINT('Ctrl Pts',(-0.24506993964978,-1.05543488480932,4.07024098687146));
#8849=CARTESIAN_POINT('Ctrl Pts',(0.353129677630186,-1.02164169574851,4.10095223014905));
#8850=CARTESIAN_POINT('Ctrl Pts',(0.840502862789607,-0.675586766930572,
4.13159054166329));
#8851=CARTESIAN_POINT('Ctrl Pts',(1.06850001744841,-0.124608973291446,4.16215528527946));
#8852=CARTESIAN_POINT('Ctrl Pts',(0.968667539921783,0.461800789232989,4.19264586113681));
#8853=CARTESIAN_POINT('Ctrl Pts',(0.573075375497625,0.904095810892864,4.22306181606733));
#8854=CARTESIAN_POINT('Ctrl Pts',(0.00428398543883978,1.06777175324867,
4.25340259677658));
#8855=CARTESIAN_POINT('Ctrl Pts',(-0.563191060635299,0.904009958454533,
4.28366811821645));
#8856=CARTESIAN_POINT('Ctrl Pts',(-0.940669220907235,0.481061734634649,
4.31273939615205));
#8857=CARTESIAN_POINT('Ctrl Pts',(-1.04748681672637,-0.0484309683621674,
4.34062676179975));
#8858=CARTESIAN_POINT('Ctrl Pts',(-0.894659216501438,-0.541420541857352,
4.3673360049139));
#8859=CARTESIAN_POINT('Ctrl Pts',(-0.464581269885186,-0.963235408380499,
4.39842750092416));
#8860=CARTESIAN_POINT('Ctrl Pts',(0.239565566362356,-1.06883033579405,4.43386078841037));
#8861=CARTESIAN_POINT('Ctrl Pts',(0.900207301627467,-0.6181471938036,4.4735881815693));
#8862=CARTESIAN_POINT('Ctrl Pts',(1.07661736077248,0.158307456468171,4.51318028163458));
#8863=CARTESIAN_POINT('Ctrl Pts',(0.679619107697134,0.845445051684285,4.55263682700741));
#8864=CARTESIAN_POINT('Ctrl Pts',(-0.0772188720163175,1.07831123772824,
4.59195908839367));
#8865=CARTESIAN_POINT('Ctrl Pts',(-0.707169488136082,0.773252871890353,
4.62679420162289));
#8866=CARTESIAN_POINT('Ctrl Pts',(-0.987518254466977,0.255555062644542,
4.65718831119431));
#8867=CARTESIAN_POINT('Ctrl Pts',(-0.987344296695494,-0.246928877186952,
4.68318021964439));
#8868=CARTESIAN_POINT('Ctrl Pts',(-0.747395974394147,-0.68790253874418,
4.70911509298375));
#8869=CARTESIAN_POINT('Ctrl Pts',(-0.326598919534621,-0.959047210599774,
4.73499264228026));
#8870=CARTESIAN_POINT('Ctrl Pts',(0.171526528910553,-0.996613146528814,
4.76081164773556));
#8871=CARTESIAN_POINT('Ctrl Pts',(0.559559675319348,-0.821106466207549,
4.78282032257176));
#8872=CARTESIAN_POINT('Ctrl Pts',(0.796278934310142,-0.570126029209407,
4.80103769428559));
#8873=CARTESIAN_POINT('Ctrl Pts',(0.964224236533784,-0.246079960768308,
4.82030349152749));
#8874=CARTESIAN_POINT('Ctrl Pts',(0.990634981866468,0.222032268895686,4.84434428541031));
#8875=CARTESIAN_POINT('Ctrl Pts',(0.718768909207029,0.713425976685633,4.87312285291378));
#8876=CARTESIAN_POINT('Ctrl Pts',(0.228511728246258,0.984171670659741,4.90183375867155));
#8877=CARTESIAN_POINT('Ctrl Pts',(-0.329439271525028,0.952675739973614,
4.93047742700953));
#8878=CARTESIAN_POINT('Ctrl Pts',(-0.784025344868638,0.629894027325748,
4.95905533359007));
#8879=CARTESIAN_POINT('Ctrl Pts',(-0.996744501476427,0.115900336236449,
4.98756854278546));
#8880=CARTESIAN_POINT('Ctrl Pts',(-0.903599797834191,-0.431268663631399,
5.01601837689846));
#8881=CARTESIAN_POINT('Ctrl Pts',(-0.534433841777186,-0.844113612462787,
5.04440611789283));
#8882=CARTESIAN_POINT('Ctrl Pts',(-0.00334246362797946,-0.996947925202839,
5.07273313603078));
#8883=CARTESIAN_POINT('Ctrl Pts',(0.526547243855696,-0.844122845511364,
5.10100084493586));
#8884=CARTESIAN_POINT('Ctrl Pts',(0.893161693859534,-0.433647847012934,
5.12921071114398));
#8885=CARTESIAN_POINT('Ctrl Pts',(0.985017050564764,0.107878463430296,5.15736425383812));
#8886=CARTESIAN_POINT('Ctrl Pts',(0.775096210047194,0.614286586251671,5.1854630337029));
#8887=CARTESIAN_POINT('Ctrl Pts',(0.328772572338644,0.930794298175775,5.21350867924155));
#8888=CARTESIAN_POINT('Ctrl Pts',(-0.216531421468218,0.961276383482143,
5.24150282972688));
#8889=CARTESIAN_POINT('Ctrl Pts',(-0.693626467566039,0.697442197976963,
5.26944723759027));
#8890=CARTESIAN_POINT('Ctrl Pts',(-0.956780044053587,0.221028354809448,
5.29734354491797));
#8891=CARTESIAN_POINT('Ctrl Pts',(-0.926194208137696,-0.321458272100224,
5.3251937796117));
#8892=CARTESIAN_POINT('Ctrl Pts',(-0.612185879018724,-0.763866525937045,
5.35299922629289));
#8893=CARTESIAN_POINT('Ctrl Pts',(-0.111725843695108,-0.971021766407051,
5.38076291905228));
#8894=CARTESIAN_POINT('Ctrl Pts',(0.421454260882621,-0.880515937840451,
5.40848407795733));
#8895=CARTESIAN_POINT('Ctrl Pts',(0.824100639480779,-0.520346924625745,
5.43617046078395));
#8896=CARTESIAN_POINT('Ctrl Pts',(0.92351355797063,-0.17546039163511,5.45459465534717));
#8897=CARTESIAN_POINT('Ctrl Pts',(0.923536902282142,-0.00205290235935909,
5.46381262547553));
#8898=CARTESIAN_POINT('Ctrl Pts',(1.02243941136618,0.00398423891480934,
2.00010574185718));
#8899=CARTESIAN_POINT('Ctrl Pts',(1.02241359427953,0.195760105709546,2.01030013552781));
#8900=CARTESIAN_POINT('Ctrl Pts',(0.912384794808815,0.57783074171643,2.03070887226764));
#8901=CARTESIAN_POINT('Ctrl Pts',(0.466210030566678,0.976979667346393,2.06138810717927));
#8902=CARTESIAN_POINT('Ctrl Pts',(-0.125096972995613,1.07745189775172,2.09213285468625));
#8903=CARTESIAN_POINT('Ctrl Pts',(-0.680513135833094,0.847598882016436,
2.1229425677617));
#8904=CARTESIAN_POINT('Ctrl Pts',(-1.02921948039241,0.35639070652297,2.15381627278417));
#8905=CARTESIAN_POINT('Ctrl Pts',(-1.06323558233127,-0.246247511674403,
2.18475313583275));
#8906=CARTESIAN_POINT('Ctrl Pts',(-0.770826846999395,-0.77569409414987,
2.21575219104532));
#8907=CARTESIAN_POINT('Ctrl Pts',(-0.240514282436741,-1.06897711434002,
2.24681248125642));
#8908=CARTESIAN_POINT('Ctrl Pts',(0.365719763837382,-1.03512322488853,2.27793292555432));
#8909=CARTESIAN_POINT('Ctrl Pts',(0.861960816498296,-0.683194362032242,
2.30911251383287));
#8910=CARTESIAN_POINT('Ctrl Pts',(1.09531889997021,-0.120271361501286,2.34034991634459));
#8911=CARTESIAN_POINT('Ctrl Pts',(0.993237192117574,0.481895386113469,2.37164430422677));
#8912=CARTESIAN_POINT('Ctrl Pts',(0.653571524566261,0.861659412057779,2.39776861909535));
#8913=CARTESIAN_POINT('Ctrl Pts',(0.291454062137944,1.02320284426481,2.41869618695453));
#8914=CARTESIAN_POINT('Ctrl Pts',(-0.00308920568304123,1.06494358035969,
2.43440512380543));
#8915=CARTESIAN_POINT('Ctrl Pts',(-0.297997185345012,1.02327054546842,2.45012728658302));
#8916=CARTESIAN_POINT('Ctrl Pts',(-0.570097692954665,0.901588560504387,
2.46586256288552));
#8917=CARTESIAN_POINT('Ctrl Pts',(-0.797915324645491,0.709118942927343,
2.48161057136306));
#8918=CARTESIAN_POINT('Ctrl Pts',(-1.00712518371007,0.396636113599795,2.50145794064213));
#8919=CARTESIAN_POINT('Ctrl Pts',(-1.08116460684588,0.0311698313189306,
2.52074077270457));
#8920=CARTESIAN_POINT('Ctrl Pts',(-1.01930513653729,-0.317331812896037,
2.5394607174683));
#8921=CARTESIAN_POINT('Ctrl Pts',(-0.874086747019434,-0.640136090368379,
2.55819302267196));
#8922=CARTESIAN_POINT('Ctrl Pts',(-0.549496069959448,-0.957169806277918,
2.58163052088621));
#8923=CARTESIAN_POINT('Ctrl Pts',(-0.0835160615693929,-1.08799952729685,
2.6066640277496));
#8924=CARTESIAN_POINT('Ctrl Pts',(0.447882551085116,-1.01298309850681,2.6348572614683));
#8925=CARTESIAN_POINT('Ctrl Pts',(0.896526797653208,-0.680517624893238,
2.66308300818814));
#8926=CARTESIAN_POINT('Ctrl Pts',(1.10361806773707,-0.107914019055422,2.69448791650807));
#8927=CARTESIAN_POINT('Ctrl Pts',(1.02236526582386,0.43282548322369,2.72278440192714));
#8928=CARTESIAN_POINT('Ctrl Pts',(0.691233446933462,0.870356607176783,2.75111176990363));
#8929=CARTESIAN_POINT('Ctrl Pts',(0.246868968583059,1.07055085263004,2.77631849214705));
#8930=CARTESIAN_POINT('Ctrl Pts',(-0.293110275260041,1.07554167301612,2.80470081460215));
#8931=CARTESIAN_POINT('Ctrl Pts',(-0.873377993524284,0.768396352809485,
2.83784367708145));
#8932=CARTESIAN_POINT('Ctrl Pts',(-1.17608632993973,-0.00167480100091063,
2.87892742744357));
#8933=CARTESIAN_POINT('Ctrl Pts',(-0.862005440846571,-0.801794854597139,
2.92164667510429));
#8934=CARTESIAN_POINT('Ctrl Pts',(-0.0868001045588601,-1.17546983264539,
2.9644142252545));
#8935=CARTESIAN_POINT('Ctrl Pts',(0.736580981803708,-0.921694810107848,
3.00722624540655));
#8936=CARTESIAN_POINT('Ctrl Pts',(1.16774349960592,-0.174918209614478,3.05007784308638));
#8937=CARTESIAN_POINT('Ctrl Pts',(0.976072265924129,0.666290888680979,3.09296369279926));
#8938=CARTESIAN_POINT('Ctrl Pts',(0.262058174942946,1.15328967289916,3.13588034038676));
#8939=CARTESIAN_POINT('Ctrl Pts',(-0.496427378766351,1.03794803578382,3.17404809518878));
#8940=CARTESIAN_POINT('Ctrl Pts',(-0.958686700933804,0.584914097624343,
3.20746239375664));
#8941=CARTESIAN_POINT('Ctrl Pts',(-1.12243569410531,0.0559111282632584,
3.23610726859073));
#8942=CARTESIAN_POINT('Ctrl Pts',(-1.01225564720179,-0.488112652692135,
3.26476379086583));
#8943=CARTESIAN_POINT('Ctrl Pts',(-0.695487043547354,-0.864710880467027,
3.29023409387107));
#8944=CARTESIAN_POINT('Ctrl Pts',(-0.205898661278593,-1.10632076377313,
3.31889882744695));
#8945=CARTESIAN_POINT('Ctrl Pts',(0.297081287657339,-1.08581158838707,3.34437380568392));
#8946=CARTESIAN_POINT('Ctrl Pts',(0.817823747991888,-0.773631518006107,
3.37622271510012));
#8947=CARTESIAN_POINT('Ctrl Pts',(1.10559906046499,-0.285197856857749,3.40488530682305));
#8948=CARTESIAN_POINT('Ctrl Pts',(1.0736525234882,0.331169973155956,3.43673056973207));
#8949=CARTESIAN_POINT('Ctrl Pts',(0.784996582513853,0.804116540088881,3.46538534226499));
#8950=CARTESIAN_POINT('Ctrl Pts',(0.304802421955024,1.08099686803911,3.49403458049713));
#8951=CARTESIAN_POINT('Ctrl Pts',(-0.341944614013262,1.098636104481,3.52745168943803));
#8952=CARTESIAN_POINT('Ctrl Pts',(-0.977091025315939,0.667069718432036,
3.56562507555433));
#8953=CARTESIAN_POINT('Ctrl Pts',(-1.13595754845858,-0.034657215805678,
3.60139104564868));
#8954=CARTESIAN_POINT('Ctrl Pts',(-0.953933695872026,-0.549739668884208,
3.62999460912882));
#8955=CARTESIAN_POINT('Ctrl Pts',(-0.687479364990766,-0.860183893070429,
3.65144052291524));
#8956=CARTESIAN_POINT('Ctrl Pts',(-0.325442973517683,-1.05119495832465,
3.67287541516038));
#8957=CARTESIAN_POINT('Ctrl Pts',(0.126139312124764,-1.10245556695548,3.69668276834371));
#8958=CARTESIAN_POINT('Ctrl Pts',(0.606262182001061,-0.941165677336213,
3.72285638725491));
#8959=CARTESIAN_POINT('Ctrl Pts',(0.981703226798656,-0.536091933987129,
3.75139484192606));
#8960=CARTESIAN_POINT('Ctrl Pts',(1.08510429065794,-0.12966335831906,3.77307496323289));
#8961=CARTESIAN_POINT('Ctrl Pts',(1.06536235673658,0.148839679722951,3.78792185774525));
#8962=CARTESIAN_POINT('Ctrl Pts',(1.02340870619934,0.345313817801113,3.79860936295049));
#8963=CARTESIAN_POINT('Ctrl Pts',(0.879143926657432,0.668877663471392,3.81730516467634));
#8964=CARTESIAN_POINT('Ctrl Pts',(0.49119057265482,1.01587840437015,3.84399122167101));
#8965=CARTESIAN_POINT('Ctrl Pts',(-0.1244886820771,1.12034446949229,3.87598677430555));
#8966=CARTESIAN_POINT('Ctrl Pts',(-0.700571603791792,0.881592069567747,
3.90794936018184));
#8967=CARTESIAN_POINT('Ctrl Pts',(-1.06104856205228,0.373416190402291,3.93987837863393));
#8968=CARTESIAN_POINT('Ctrl Pts',(-1.09581923957444,-0.247931090158792,
3.97177133910303));
#8969=CARTESIAN_POINT('Ctrl Pts',(-0.795058502865452,-0.791907253963627,
4.00362670823387));
#8970=CARTESIAN_POINT('Ctrl Pts',(-0.251647494919828,-1.09210956787375,
4.03544259599333));
#8971=CARTESIAN_POINT('Ctrl Pts',(0.367379394643827,-1.05723105471296,4.06721734153362));
#8972=CARTESIAN_POINT('Ctrl Pts',(0.872287547395435,-0.698834410234474,
4.09894925108463));
#8973=CARTESIAN_POINT('Ctrl Pts',(1.10877998781386,-0.127551616843013,4.13063668619542));
#8974=CARTESIAN_POINT('Ctrl Pts',(1.0052446536512,0.481111111451165,4.16227808117121));
#8975=CARTESIAN_POINT('Ctrl Pts',(0.594321870531113,0.940669990088406,4.1938717879661));
#8976=CARTESIAN_POINT('Ctrl Pts',(0.0028836137700018,1.11094669369995,4.2254164735472));
#8977=CARTESIAN_POINT('Ctrl Pts',(-0.587756102544925,0.940586366285575,
4.25691019880358));
#8978=CARTESIAN_POINT('Ctrl Pts',(-0.98100418266937,0.500061769547605,4.28718787478163));
#8979=CARTESIAN_POINT('Ctrl Pts',(-1.0924189681305,-0.0518986088236793,
4.31625322570434));
#8980=CARTESIAN_POINT('Ctrl Pts',(-0.932995695727251,-0.566234439465872,
4.34411668254595));
#8981=CARTESIAN_POINT('Ctrl Pts',(-0.484070307765096,-1.00664758476799,
4.37657109924072));
#8982=CARTESIAN_POINT('Ctrl Pts',(0.251603665111017,-1.1170577608396,4.41358577518597));
#8983=CARTESIAN_POINT('Ctrl Pts',(0.942532607043053,-0.645899595864585,
4.45512260600759));
#8984=CARTESIAN_POINT('Ctrl Pts',(1.12727625401763,0.166757495434457,4.4965526452627));
#8985=CARTESIAN_POINT('Ctrl Pts',(0.711535392414827,0.886568160592581,4.53787467403547));
#8986=CARTESIAN_POINT('Ctrl Pts',(-0.0817754479350662,1.13077645625679,
4.57908545141459));
#8987=CARTESIAN_POINT('Ctrl Pts',(-0.742544779926902,0.810887680269329,
4.61561571764965));
#8988=CARTESIAN_POINT('Ctrl Pts',(-1.0367889170548,0.267632475490702,4.64750621726079));
#8989=CARTESIAN_POINT('Ctrl Pts',(-1.03661273079663,-0.259890812374001,
4.67479142272022));
#8990=CARTESIAN_POINT('Ctrl Pts',(-0.784674395084709,-0.722985135309321,
4.70202319451165));
#8991=CARTESIAN_POINT('Ctrl Pts',(-0.342665105846928,-1.0078013893598,4.72920190577311));
#8992=CARTESIAN_POINT('Ctrl Pts',(0.180728280565742,-1.04730098586176,4.75632941787614));
#8993=CARTESIAN_POINT('Ctrl Pts',(0.588474355690808,-0.862865648071463,
4.77945118635523));
#8994=CARTESIAN_POINT('Ctrl Pts',(0.837298510008721,-0.599056189202392,
4.79859890763443));
#8995=CARTESIAN_POINT('Ctrl Pts',(1.01384364614042,-0.258411401611501,4.81884983955842));
#8996=CARTESIAN_POINT('Ctrl Pts',(1.04161074189106,0.233686771419479,4.84411811105277));
#8997=CARTESIAN_POINT('Ctrl Pts',(0.755768464274831,0.75035189256676,4.87437275136583));
#8998=CARTESIAN_POINT('Ctrl Pts',(0.240260832126417,1.03503398641502,4.90455785690813));
#8999=CARTESIAN_POINT('Ctrl Pts',(-0.346443076772766,1.00191052777563,4.93467391487705));
#9000=CARTESIAN_POINT('Ctrl Pts',(-0.824443961186794,0.662491998876826,
4.96472035161675));
#9001=CARTESIAN_POINT('Ctrl Pts',(-1.04809749408919,0.122047597909646,4.99469718541711));
#9002=CARTESIAN_POINT('Ctrl Pts',(-0.950155996017736,-0.453210166677515,
5.02460427322952));
#9003=CARTESIAN_POINT('Ctrl Pts',(-0.562083374811871,-0.887170351531481,
5.05444164408033));
#9004=CARTESIAN_POINT('Ctrl Pts',(-0.00391861514886455,-1.04777194538233,
5.08420934418352));
#9005=CARTESIAN_POINT('Ctrl Pts',(0.552831610598961,-0.887172147683135,
5.11390750584928));
#9006=CARTESIAN_POINT('Ctrl Pts',(0.937898903203791,-0.455990569053019,
5.14353631321098));
#9007=CARTESIAN_POINT('Ctrl Pts',(1.03431638593341,0.112638134192545,5.17309601934115));
#9008=CARTESIAN_POINT('Ctrl Pts',(0.813941584329194,0.644164866246659,5.20258693124811));
#9009=CARTESIAN_POINT('Ctrl Pts',(0.345645707405533,0.976202338133972,5.23200943013856));
#9010=CARTESIAN_POINT('Ctrl Pts',(-0.226201062045275,1.0081223330431,5.26136393052504));
#9011=CARTESIAN_POINT('Ctrl Pts',(-0.726229018344627,0.731549687209916,
5.29065096134688));
#9012=CARTESIAN_POINT('Ctrl Pts',(-1.0018409132178,0.232472985169518,5.31987098313559));
#9013=CARTESIAN_POINT('Ctrl Pts',(-0.969765726171833,-0.335436557731811,
5.34902478961936));
#9014=CARTESIAN_POINT('Ctrl Pts',(-0.64121170398132,-0.798235214103243,
5.378112596859));
#9015=CARTESIAN_POINT('Ctrl Pts',(-0.117992925426973,-1.01474627932904,
5.40713604807643));
#9016=CARTESIAN_POINT('Ctrl Pts',(0.438971330353334,-0.9201244737966,5.43609371817436));
#9017=CARTESIAN_POINT('Ctrl Pts',(0.859207049494131,-0.544141904102835,
5.46499108972057));
#9018=CARTESIAN_POINT('Ctrl Pts',(0.962831133440289,-0.184383467346616,
5.48420765452691));
#9019=CARTESIAN_POINT('Ctrl Pts',(0.962855463572385,-0.00365305179164034,
5.49381489570681));
#9020=CARTESIAN_POINT('Ctrl Pts',(0.999999464043874,0.00398121802342207,
2.00010574185718));
#9021=CARTESIAN_POINT('Ctrl Pts',(0.999974206061282,0.19160391813607,2.01007936209659));
#9022=CARTESIAN_POINT('Ctrl Pts',(0.892358674149497,0.565284907029969,2.03003975780563));
#9023=CARTESIAN_POINT('Ctrl Pts',(0.455908354460267,0.955754980387012,2.06005123671475));
#9024=CARTESIAN_POINT('Ctrl Pts',(-0.122563158588718,1.05404138225222,2.09012808179557));
#9025=CARTESIAN_POINT('Ctrl Pts',(-0.665982422429721,0.829161410069987,
2.12027227517451));
#9026=CARTESIAN_POINT('Ctrl Pts',(-1.00720268117277,0.348508238874394,2.15048257508427));
#9027=CARTESIAN_POINT('Ctrl Pts',(-1.04050120808252,-0.241264621011279,
2.18075912672908));
#9028=CARTESIAN_POINT('Ctrl Pts',(-0.754298406118339,-0.759496345182109,
2.21110138862918));
#9029=CARTESIAN_POINT('Ctrl Pts',(-0.235139085598783,-1.04662471701868,
2.24150905560043));
#9030=CARTESIAN_POINT('Ctrl Pts',(0.358466657407177,-1.0134893307861,2.27198163744466));
#9031=CARTESIAN_POINT('Ctrl Pts',(0.844481314225998,-0.668830870873697,
2.30251864881201));
#9032=CARTESIAN_POINT('Ctrl Pts',(1.07309171546203,-0.117397710656463,2.33311952120739));
#9033=CARTESIAN_POINT('Ctrl Pts',(0.973085863935879,0.472631726678538,2.36378364003101));
#9034=CARTESIAN_POINT('Ctrl Pts',(0.640186615940372,0.844850208282888,2.38938921676183));
#9035=CARTESIAN_POINT('Ctrl Pts',(0.285207254948024,1.00321211946817,2.40990460122644));
#9036=CARTESIAN_POINT('Ctrl Pts',(-0.00357278466147455,1.04413748919053,
2.42530650345941));
#9037=CARTESIAN_POINT('Ctrl Pts',(-0.292753333069628,1.00327492007872,2.4407236705559));
#9038=CARTESIAN_POINT('Ctrl Pts',(-0.559610149845377,0.883939984413932,
2.45615599894115));
#9039=CARTESIAN_POINT('Ctrl Pts',(-0.783072629292576,0.695150535469123,
2.47160338259101));
#9040=CARTESIAN_POINT('Ctrl Pts',(-0.9883155178948,0.388599518613216,2.49107446360262));
#9041=CARTESIAN_POINT('Ctrl Pts',(-1.06097928852007,0.0299698265249316,
2.50999804459158));
#9042=CARTESIAN_POINT('Ctrl Pts',(-1.00026874085688,-0.31207309433285,2.52837129391011));
#9043=CARTESIAN_POINT('Ctrl Pts',(-0.85772117693898,-0.628943233787528,
2.54675983289627));
#9044=CARTESIAN_POINT('Ctrl Pts',(-0.539023756454129,-0.940248430945502,
2.56977396086322));
#9045=CARTESIAN_POINT('Ctrl Pts',(-0.0813539710712336,-1.06875629404709,
2.59436218564022));
#9046=CARTESIAN_POINT('Ctrl Pts',(0.440709506996878,-0.995074461032676,
2.6220606386953));
#9047=CARTESIAN_POINT('Ctrl Pts',(0.881652173543376,-0.668351901468915,
2.64980261114177));
#9048=CARTESIAN_POINT('Ctrl Pts',(1.0852948664173,-0.105373203004237,2.68068203601616));
#9049=CARTESIAN_POINT('Ctrl Pts',(1.00539530848997,0.426480980519131,2.70851510392812));
#9050=CARTESIAN_POINT('Ctrl Pts',(0.679609573339881,0.857002336026301,2.7363888804944));
#9051=CARTESIAN_POINT('Ctrl Pts',(0.242228396206659,1.05406947259606,2.76120094819001));
#9052=CARTESIAN_POINT('Ctrl Pts',(-0.289433825273236,1.05900157503401,2.78914691397882));
#9053=CARTESIAN_POINT('Ctrl Pts',(-0.861030373991185,0.756502517113054,
2.82179513727801));
#9054=CARTESIAN_POINT('Ctrl Pts',(-1.15948386741598,-0.00245881106342116,
2.8622922968233));
#9055=CARTESIAN_POINT('Ctrl Pts',(-0.849819252545902,-0.791606149879273,
2.9044266522989));
#9056=CARTESIAN_POINT('Ctrl Pts',(-0.0848273064559805,-1.16047682132822,
2.94663705560064));
#9057=CARTESIAN_POINT('Ctrl Pts',(0.728338616139595,-0.909963609903424,
2.98891980674896));
#9058=CARTESIAN_POINT('Ctrl Pts',(1.15452570093491,-0.172022292800125,3.03127110274204));
#9059=CARTESIAN_POINT('Ctrl Pts',(0.965079959728901,0.659906484623926,3.07368702284038));
#9060=CARTESIAN_POINT('Ctrl Pts',(0.258512451458961,1.14196808324737,3.11616354351132));
#9061=CARTESIAN_POINT('Ctrl Pts',(-0.492717397384934,1.02781794268986,3.15397066853381));
#9062=CARTESIAN_POINT('Ctrl Pts',(-0.950847731766782,0.578891230696036,
3.18708578741999));
#9063=CARTESIAN_POINT('Ctrl Pts',(-1.11322603418831,0.0543699563964829,
3.21549214280387));
#9064=CARTESIAN_POINT('Ctrl Pts',(-1.00397682800075,-0.485299668185688,
3.24391918371992));
#9065=CARTESIAN_POINT('Ctrl Pts',(-0.689560596566738,-0.85912025786842,
3.2692049003822));
#9066=CARTESIAN_POINT('Ctrl Pts',(-0.203462101275883,-1.09903917913844,
3.29766639858301));
#9067=CARTESIAN_POINT('Ctrl Pts',(0.296274556510708,-1.07870085350966,3.32298079518316));
#9068=CARTESIAN_POINT('Ctrl Pts',(0.813909810244539,-0.768416856681802,
3.35464092662437));
#9069=CARTESIAN_POINT('Ctrl Pts',(1.10016251506307,-0.282678926353398,3.38314956983213));
#9070=CARTESIAN_POINT('Ctrl Pts',(1.06842542005047,0.330699838209083,3.41484232929802));
#9071=CARTESIAN_POINT('Ctrl Pts',(0.781036889262004,0.801635745996559,3.44337716794684));
#9072=CARTESIAN_POINT('Ctrl Pts',(0.3026681656048,1.07751158150631,3.47192198965488));
#9073=CARTESIAN_POINT('Ctrl Pts',(-0.341977208139237,1.09513778685306,3.5052343169007));
#9074=CARTESIAN_POINT('Ctrl Pts',(-0.975597618652369,0.664760099314692,
3.54331757606612));
#9075=CARTESIAN_POINT('Ctrl Pts',(-1.13429370842399,-0.0357778387848846,
3.57903024860792));
#9076=CARTESIAN_POINT('Ctrl Pts',(-0.952497172320662,-0.550291907933128,
3.60760379990449));
#9077=CARTESIAN_POINT('Ctrl Pts',(-0.68624513734708,-0.860512981218381,
3.62903507783467));
#9078=CARTESIAN_POINT('Ctrl Pts',(-0.324306798008731,-1.0514860754467,3.65046688028005));
#9079=CARTESIAN_POINT('Ctrl Pts',(0.127344232453658,-1.10276625857497,3.674279919598));
#9080=CARTESIAN_POINT('Ctrl Pts',(0.607784221866902,-0.941400265606059,
3.70047332316486));
#9081=CARTESIAN_POINT('Ctrl Pts',(0.983690388895233,-0.535896868540009,
3.72904537472281));
#9082=CARTESIAN_POINT('Ctrl Pts',(1.08731538430027,-0.128732018548745,3.75076902067426));
#9083=CARTESIAN_POINT('Ctrl Pts',(1.06753777509939,0.150334725456009,3.7656464393213));
#9084=CARTESIAN_POINT('Ctrl Pts',(1.02549367550628,0.347236435696266,3.7763575734054));
#9085=CARTESIAN_POINT('Ctrl Pts',(0.880884191480398,0.671592660752369,3.7951003560531));
#9086=CARTESIAN_POINT('Ctrl Pts',(0.491799935626419,1.0196644890383,3.82187027476111));
#9087=CARTESIAN_POINT('Ctrl Pts',(-0.126065746592581,1.12455786056488,3.85398342973913));
#9088=CARTESIAN_POINT('Ctrl Pts',(-0.704583522010695,0.88486307777345,3.88608387297236));
#9089=CARTESIAN_POINT('Ctrl Pts',(-1.06683466983354,0.3742832244399,3.91816964977168));
#9090=CARTESIAN_POINT('Ctrl Pts',(-1.10184933977514,-0.250419432627018,
3.95023881727803));
#9091=CARTESIAN_POINT('Ctrl Pts',(-0.799326718711519,-0.797694380880393,
3.98228945733906));
#9092=CARTESIAN_POINT('Ctrl Pts',(-0.252343111177166,-1.09993153075449,
4.01431965364637));
#9093=CARTESIAN_POINT('Ctrl Pts',(0.371159169345164,-1.06485412373635,4.0463275194738));
#9094=CARTESIAN_POINT('Ctrl Pts',(0.880047504125487,-0.703696890362346,
4.07831118189475));
#9095=CARTESIAN_POINT('Ctrl Pts',(1.11857837754389,-0.127626743256515,4.11026879475596));
#9096=CARTESIAN_POINT('Ctrl Pts',(1.01416153614381,0.486524030990474,4.14219853012843));
#9097=CARTESIAN_POINT('Ctrl Pts',(0.599338058827864,0.950520440175857,4.17409858361638));
#9098=CARTESIAN_POINT('Ctrl Pts',(0.00190308953361062,1.12257447034417,
4.20596718959497));
#9099=CARTESIAN_POINT('Ctrl Pts',(-0.595087816877256,0.950429978912684,
4.23780259148061));
#9100=CARTESIAN_POINT('Ctrl Pts',(-0.992818074176864,0.504960206465758,
4.26842528448615));
#9101=CARTESIAN_POINT('Ctrl Pts',(-1.10558192615926,-0.0535255134762696,
4.29783816996833));
#9102=CARTESIAN_POINT('Ctrl Pts',(-0.944245633155887,-0.574182433998452,
4.326044460862));
#9103=CARTESIAN_POINT('Ctrl Pts',(-0.489615552103502,-1.02023046107543,
4.35891537170686));
#9104=CARTESIAN_POINT('Ctrl Pts',(0.255873406558148,-1.13223620757883,4.39642822383059));
#9105=CARTESIAN_POINT('Ctrl Pts',(0.956585537399415,-0.654531370431507,
4.43855371945495));
#9106=CARTESIAN_POINT('Ctrl Pts',(1.14416456861692,0.170066871142059,4.48059920430672));
#9107=CARTESIAN_POINT('Ctrl Pts',(0.722117099067864,0.901002181388938,4.52256123999552));
#9108=CARTESIAN_POINT('Ctrl Pts',(-0.0838676738781217,1.14921441407926,
4.5644365266184));
#9109=CARTESIAN_POINT('Ctrl Pts',(-0.755677502986392,0.824069849946143,
4.60157908243497));
#9110=CARTESIAN_POINT('Ctrl Pts',(-1.05498104408691,0.271521112381307,4.63401858831428));
#9111=CARTESIAN_POINT('Ctrl Pts',(-1.05483403133078,-0.26522135570406,4.66178172056988));
#9112=CARTESIAN_POINT('Ctrl Pts',(-0.79840547489227,-0.736599185468657,
4.68950186792131));
#9113=CARTESIAN_POINT('Ctrl Pts',(-0.3483499377511,-1.02663834291108,4.71717822726345));
#9114=CARTESIAN_POINT('Ctrl Pts',(0.184757632451299,-1.06688722115596,4.74481003558103));
#9115=CARTESIAN_POINT('Ctrl Pts',(0.600256695779753,-0.878980608467174,
4.7683735201888));
#9116=CARTESIAN_POINT('Ctrl Pts',(0.853850233649786,-0.610120445383555,
4.78788851920089));
#9117=CARTESIAN_POINT('Ctrl Pts',(1.03381570897682,-0.262894148472765,4.80853189587555));
#9118=CARTESIAN_POINT('Ctrl Pts',(1.06215687349528,0.238874309450968,4.83429913779336));
#9119=CARTESIAN_POINT('Ctrl Pts',(0.770634803840811,0.765869068483215,4.86515976481244));
#9120=CARTESIAN_POINT('Ctrl Pts',(0.244684747552399,1.05635550605388,4.89595947659513));
#9121=CARTESIAN_POINT('Ctrl Pts',(-0.354100647382748,1.02257824395859,4.92669748292077));
#9122=CARTESIAN_POINT('Ctrl Pts',(-0.842095960257555,0.676096127224308,
4.95737304397893));
#9123=CARTESIAN_POINT('Ctrl Pts',(-1.07050216965279,0.124232350128257,4.98798547954758));
#9124=CARTESIAN_POINT('Ctrl Pts',(-0.970487698233666,-0.463339790807337,
5.01853416178037));
#9125=CARTESIAN_POINT('Ctrl Pts',(-0.57403535125674,-0.906703305752076,
5.04901852189829));
#9126=CARTESIAN_POINT('Ctrl Pts',(-0.00367933936324437,-1.07083384017741,
5.07943804916124));
#9127=CARTESIAN_POINT('Ctrl Pts',(0.56535226719551,-0.906710964597204,5.10979228847672));
#9128=CARTESIAN_POINT('Ctrl Pts',(0.95899197878984,-0.465956326824321,5.14008084401914));
#9129=CARTESIAN_POINT('Ctrl Pts',(1.05758360680831,0.115400410376887,5.17030337915801));
#9130=CARTESIAN_POINT('Ctrl Pts',(0.832257130959616,0.658907139635372,5.20045961311858));
#9131=CARTESIAN_POINT('Ctrl Pts',(0.353362036446966,0.998475173781019,5.23054933034559));
#9132=CARTESIAN_POINT('Ctrl Pts',(-0.231493376683462,1.03113233690688,5.26057235733975));
#9133=CARTESIAN_POINT('Ctrl Pts',(-0.742941371583914,0.748253733713579,
5.29052861685377));
#9134=CARTESIAN_POINT('Ctrl Pts',(-1.02486870130036,0.23775759542928,5.3204180022368));
#9135=CARTESIAN_POINT('Ctrl Pts',(-0.992064317380329,-0.343173817499407,
5.3502406538254));
#9136=CARTESIAN_POINT('Ctrl Pts',(-0.655975229859479,-0.81659286891466,
5.37999633599993));
#9137=CARTESIAN_POINT('Ctrl Pts',(-0.120753665413257,-1.03807600951265,
5.40968580999697));
#9138=CARTESIAN_POINT('Ctrl Pts',(0.44897427078276,-0.941278849111864,5.43930775328404));
#9139=CARTESIAN_POINT('Ctrl Pts',(0.878820594563222,-0.556707495126734,
5.46886560818098));
#9140=CARTESIAN_POINT('Ctrl Pts',(0.984806813297395,-0.188706783169536,
5.48852259094232));
#9141=CARTESIAN_POINT('Ctrl Pts',(0.984831692610592,-0.00389691057600537,
5.49834668730695));
#9142=CARTESIAN_POINT('',(0.999999464043874,0.00398121802342206,2.00010574185718));
#9143=CARTESIAN_POINT('Origin',(1.,0.,2.075));
#9144=CARTESIAN_POINT('',(0.984831692610592,-0.00389691057600538,5.49834668730695));
#9145=CARTESIAN_POINT('Ctrl Pts',(0.999999464043874,0.00398121802342207,
2.00010574185718));
#9146=CARTESIAN_POINT('Ctrl Pts',(0.999974206061282,0.19160391813607,2.01007936209659));
#9147=CARTESIAN_POINT('Ctrl Pts',(0.892358674149497,0.565284907029969,2.03003975780563));
#9148=CARTESIAN_POINT('Ctrl Pts',(0.455908354460267,0.955754980387012,2.06005123671475));
#9149=CARTESIAN_POINT('Ctrl Pts',(-0.122563158588718,1.05404138225222,2.09012808179557));
#9150=CARTESIAN_POINT('Ctrl Pts',(-0.665982422429721,0.829161410069987,
2.12027227517451));
#9151=CARTESIAN_POINT('Ctrl Pts',(-1.00720268117277,0.348508238874394,2.15048257508427));
#9152=CARTESIAN_POINT('Ctrl Pts',(-1.04050120808252,-0.241264621011279,
2.18075912672908));
#9153=CARTESIAN_POINT('Ctrl Pts',(-0.754298406118339,-0.759496345182109,
2.21110138862918));
#9154=CARTESIAN_POINT('Ctrl Pts',(-0.235139085598783,-1.04662471701868,
2.24150905560043));
#9155=CARTESIAN_POINT('Ctrl Pts',(0.358466657407177,-1.0134893307861,2.27198163744466));
#9156=CARTESIAN_POINT('Ctrl Pts',(0.844481314225998,-0.668830870873697,
2.30251864881201));
#9157=CARTESIAN_POINT('Ctrl Pts',(1.07309171546203,-0.117397710656463,2.33311952120739));
#9158=CARTESIAN_POINT('Ctrl Pts',(0.973085863935879,0.472631726678538,2.36378364003101));
#9159=CARTESIAN_POINT('Ctrl Pts',(0.640186615940372,0.844850208282888,2.38938921676183));
#9160=CARTESIAN_POINT('Ctrl Pts',(0.285207254948024,1.00321211946817,2.40990460122644));
#9161=CARTESIAN_POINT('Ctrl Pts',(-0.00357278466147455,1.04413748919053,
2.42530650345941));
#9162=CARTESIAN_POINT('Ctrl Pts',(-0.292753333069628,1.00327492007872,2.4407236705559));
#9163=CARTESIAN_POINT('Ctrl Pts',(-0.559610149845377,0.883939984413932,
2.45615599894115));
#9164=CARTESIAN_POINT('Ctrl Pts',(-0.783072629292576,0.695150535469123,
2.47160338259101));
#9165=CARTESIAN_POINT('Ctrl Pts',(-0.9883155178948,0.388599518613216,2.49107446360262));
#9166=CARTESIAN_POINT('Ctrl Pts',(-1.06097928852007,0.0299698265249316,
2.50999804459158));
#9167=CARTESIAN_POINT('Ctrl Pts',(-1.00026874085688,-0.31207309433285,2.52837129391011));
#9168=CARTESIAN_POINT('Ctrl Pts',(-0.85772117693898,-0.628943233787528,
2.54675983289627));
#9169=CARTESIAN_POINT('Ctrl Pts',(-0.539023756454129,-0.940248430945502,
2.56977396086322));
#9170=CARTESIAN_POINT('Ctrl Pts',(-0.0813539710712336,-1.06875629404709,
2.59436218564022));
#9171=CARTESIAN_POINT('Ctrl Pts',(0.440709506996878,-0.995074461032676,
2.6220606386953));
#9172=CARTESIAN_POINT('Ctrl Pts',(0.881652173543376,-0.668351901468915,
2.64980261114177));
#9173=CARTESIAN_POINT('Ctrl Pts',(1.0852948664173,-0.105373203004237,2.68068203601616));
#9174=CARTESIAN_POINT('Ctrl Pts',(1.00539530848997,0.426480980519131,2.70851510392812));
#9175=CARTESIAN_POINT('Ctrl Pts',(0.679609573339881,0.857002336026301,2.7363888804944));
#9176=CARTESIAN_POINT('Ctrl Pts',(0.242228396206659,1.05406947259606,2.76120094819001));
#9177=CARTESIAN_POINT('Ctrl Pts',(-0.289433825273236,1.05900157503401,2.78914691397882));
#9178=CARTESIAN_POINT('Ctrl Pts',(-0.861030373991185,0.756502517113054,
2.82179513727801));
#9179=CARTESIAN_POINT('Ctrl Pts',(-1.15948386741598,-0.00245881106342116,
2.8622922968233));
#9180=CARTESIAN_POINT('Ctrl Pts',(-0.849819252545902,-0.791606149879273,
2.9044266522989));
#9181=CARTESIAN_POINT('Ctrl Pts',(-0.0848273064559805,-1.16047682132822,
2.94663705560064));
#9182=CARTESIAN_POINT('Ctrl Pts',(0.728338616139595,-0.909963609903424,
2.98891980674896));
#9183=CARTESIAN_POINT('Ctrl Pts',(1.15452570093491,-0.172022292800125,3.03127110274204));
#9184=CARTESIAN_POINT('Ctrl Pts',(0.965079959728901,0.659906484623926,3.07368702284038));
#9185=CARTESIAN_POINT('Ctrl Pts',(0.258512451458961,1.14196808324737,3.11616354351132));
#9186=CARTESIAN_POINT('Ctrl Pts',(-0.492717397384934,1.02781794268986,3.15397066853381));
#9187=CARTESIAN_POINT('Ctrl Pts',(-0.950847731766782,0.578891230696036,
3.18708578741999));
#9188=CARTESIAN_POINT('Ctrl Pts',(-1.11322603418831,0.0543699563964829,
3.21549214280387));
#9189=CARTESIAN_POINT('Ctrl Pts',(-1.00397682800075,-0.485299668185688,
3.24391918371992));
#9190=CARTESIAN_POINT('Ctrl Pts',(-0.689560596566738,-0.85912025786842,
3.2692049003822));
#9191=CARTESIAN_POINT('Ctrl Pts',(-0.203462101275883,-1.09903917913844,
3.29766639858301));
#9192=CARTESIAN_POINT('Ctrl Pts',(0.296274556510708,-1.07870085350966,3.32298079518316));
#9193=CARTESIAN_POINT('Ctrl Pts',(0.813909810244539,-0.768416856681802,
3.35464092662437));
#9194=CARTESIAN_POINT('Ctrl Pts',(1.10016251506307,-0.282678926353398,3.38314956983213));
#9195=CARTESIAN_POINT('Ctrl Pts',(1.06842542005047,0.330699838209083,3.41484232929802));
#9196=CARTESIAN_POINT('Ctrl Pts',(0.781036889262004,0.801635745996559,3.44337716794684));
#9197=CARTESIAN_POINT('Ctrl Pts',(0.3026681656048,1.07751158150631,3.47192198965488));
#9198=CARTESIAN_POINT('Ctrl Pts',(-0.341977208139237,1.09513778685306,3.5052343169007));
#9199=CARTESIAN_POINT('Ctrl Pts',(-0.975597618652369,0.664760099314692,
3.54331757606612));
#9200=CARTESIAN_POINT('Ctrl Pts',(-1.13429370842399,-0.0357778387848846,
3.57903024860792));
#9201=CARTESIAN_POINT('Ctrl Pts',(-0.952497172320662,-0.550291907933128,
3.60760379990449));
#9202=CARTESIAN_POINT('Ctrl Pts',(-0.68624513734708,-0.860512981218381,
3.62903507783467));
#9203=CARTESIAN_POINT('Ctrl Pts',(-0.324306798008731,-1.0514860754467,3.65046688028005));
#9204=CARTESIAN_POINT('Ctrl Pts',(0.127344232453658,-1.10276625857497,3.674279919598));
#9205=CARTESIAN_POINT('Ctrl Pts',(0.607784221866902,-0.941400265606059,
3.70047332316486));
#9206=CARTESIAN_POINT('Ctrl Pts',(0.983690388895233,-0.535896868540009,
3.72904537472281));
#9207=CARTESIAN_POINT('Ctrl Pts',(1.08731538430027,-0.128732018548745,3.75076902067426));
#9208=CARTESIAN_POINT('Ctrl Pts',(1.06753777509939,0.150334725456009,3.7656464393213));
#9209=CARTESIAN_POINT('Ctrl Pts',(1.02549367550628,0.347236435696266,3.7763575734054));
#9210=CARTESIAN_POINT('Ctrl Pts',(0.880884191480398,0.671592660752369,3.7951003560531));
#9211=CARTESIAN_POINT('Ctrl Pts',(0.491799935626419,1.0196644890383,3.82187027476111));
#9212=CARTESIAN_POINT('Ctrl Pts',(-0.126065746592581,1.12455786056488,3.85398342973913));
#9213=CARTESIAN_POINT('Ctrl Pts',(-0.704583522010695,0.88486307777345,3.88608387297236));
#9214=CARTESIAN_POINT('Ctrl Pts',(-1.06683466983354,0.3742832244399,3.91816964977168));
#9215=CARTESIAN_POINT('Ctrl Pts',(-1.10184933977514,-0.250419432627018,
3.95023881727803));
#9216=CARTESIAN_POINT('Ctrl Pts',(-0.799326718711519,-0.797694380880393,
3.98228945733906));
#9217=CARTESIAN_POINT('Ctrl Pts',(-0.252343111177166,-1.09993153075449,
4.01431965364637));
#9218=CARTESIAN_POINT('Ctrl Pts',(0.371159169345164,-1.06485412373635,4.0463275194738));
#9219=CARTESIAN_POINT('Ctrl Pts',(0.880047504125487,-0.703696890362346,
4.07831118189475));
#9220=CARTESIAN_POINT('Ctrl Pts',(1.11857837754389,-0.127626743256515,4.11026879475596));
#9221=CARTESIAN_POINT('Ctrl Pts',(1.01416153614381,0.486524030990474,4.14219853012843));
#9222=CARTESIAN_POINT('Ctrl Pts',(0.599338058827864,0.950520440175857,4.17409858361638));
#9223=CARTESIAN_POINT('Ctrl Pts',(0.00190308953361062,1.12257447034417,
4.20596718959497));
#9224=CARTESIAN_POINT('Ctrl Pts',(-0.595087816877256,0.950429978912684,
4.23780259148061));
#9225=CARTESIAN_POINT('Ctrl Pts',(-0.992818074176864,0.504960206465758,
4.26842528448615));
#9226=CARTESIAN_POINT('Ctrl Pts',(-1.10558192615926,-0.0535255134762696,
4.29783816996833));
#9227=CARTESIAN_POINT('Ctrl Pts',(-0.944245633155887,-0.574182433998452,
4.326044460862));
#9228=CARTESIAN_POINT('Ctrl Pts',(-0.489615552103502,-1.02023046107543,
4.35891537170686));
#9229=CARTESIAN_POINT('Ctrl Pts',(0.255873406558148,-1.13223620757883,4.39642822383059));
#9230=CARTESIAN_POINT('Ctrl Pts',(0.956585537399415,-0.654531370431507,
4.43855371945495));
#9231=CARTESIAN_POINT('Ctrl Pts',(1.14416456861692,0.170066871142059,4.48059920430672));
#9232=CARTESIAN_POINT('Ctrl Pts',(0.722117099067864,0.901002181388938,4.52256123999552));
#9233=CARTESIAN_POINT('Ctrl Pts',(-0.0838676738781217,1.14921441407926,
4.5644365266184));
#9234=CARTESIAN_POINT('Ctrl Pts',(-0.755677502986392,0.824069849946143,
4.60157908243497));
#9235=CARTESIAN_POINT('Ctrl Pts',(-1.05498104408691,0.271521112381307,4.63401858831428));
#9236=CARTESIAN_POINT('Ctrl Pts',(-1.05483403133078,-0.26522135570406,4.66178172056988));
#9237=CARTESIAN_POINT('Ctrl Pts',(-0.79840547489227,-0.736599185468657,
4.68950186792131));
#9238=CARTESIAN_POINT('Ctrl Pts',(-0.3483499377511,-1.02663834291108,4.71717822726345));
#9239=CARTESIAN_POINT('Ctrl Pts',(0.184757632451299,-1.06688722115596,4.74481003558103));
#9240=CARTESIAN_POINT('Ctrl Pts',(0.600256695779753,-0.878980608467174,
4.7683735201888));
#9241=CARTESIAN_POINT('Ctrl Pts',(0.853850233649786,-0.610120445383555,
4.78788851920089));
#9242=CARTESIAN_POINT('Ctrl Pts',(1.03381570897682,-0.262894148472765,4.80853189587555));
#9243=CARTESIAN_POINT('Ctrl Pts',(1.06215687349528,0.238874309450968,4.83429913779336));
#9244=CARTESIAN_POINT('Ctrl Pts',(0.770634803840811,0.765869068483215,4.86515976481244));
#9245=CARTESIAN_POINT('Ctrl Pts',(0.244684747552399,1.05635550605388,4.89595947659513));
#9246=CARTESIAN_POINT('Ctrl Pts',(-0.354100647382748,1.02257824395859,4.92669748292077));
#9247=CARTESIAN_POINT('Ctrl Pts',(-0.842095960257555,0.676096127224308,
4.95737304397893));
#9248=CARTESIAN_POINT('Ctrl Pts',(-1.07050216965279,0.124232350128257,4.98798547954758));
#9249=CARTESIAN_POINT('Ctrl Pts',(-0.970487698233666,-0.463339790807337,
5.01853416178037));
#9250=CARTESIAN_POINT('Ctrl Pts',(-0.57403535125674,-0.906703305752076,
5.04901852189829));
#9251=CARTESIAN_POINT('Ctrl Pts',(-0.00367933936324437,-1.07083384017741,
5.07943804916124));
#9252=CARTESIAN_POINT('Ctrl Pts',(0.56535226719551,-0.906710964597204,5.10979228847672));
#9253=CARTESIAN_POINT('Ctrl Pts',(0.95899197878984,-0.465956326824321,5.14008084401914));
#9254=CARTESIAN_POINT('Ctrl Pts',(1.05758360680831,0.115400410376887,5.17030337915801));
#9255=CARTESIAN_POINT('Ctrl Pts',(0.832257130959616,0.658907139635372,5.20045961311858));
#9256=CARTESIAN_POINT('Ctrl Pts',(0.353362036446966,0.998475173781019,5.23054933034559));
#9257=CARTESIAN_POINT('Ctrl Pts',(-0.231493376683462,1.03113233690688,5.26057235733975));
#9258=CARTESIAN_POINT('Ctrl Pts',(-0.742941371583914,0.748253733713579,
5.29052861685377));
#9259=CARTESIAN_POINT('Ctrl Pts',(-1.02486870130036,0.23775759542928,5.3204180022368));
#9260=CARTESIAN_POINT('Ctrl Pts',(-0.992064317380329,-0.343173817499407,
5.3502406538254));
#9261=CARTESIAN_POINT('Ctrl Pts',(-0.655975229859479,-0.81659286891466,
5.37999633599993));
#9262=CARTESIAN_POINT('Ctrl Pts',(-0.120753665413257,-1.03807600951265,
5.40968580999697));
#9263=CARTESIAN_POINT('Ctrl Pts',(0.44897427078276,-0.941278849111864,5.43930775328404));
#9264=CARTESIAN_POINT('Ctrl Pts',(0.878820594563222,-0.556707495126734,
5.46886560818098));
#9265=CARTESIAN_POINT('Ctrl Pts',(0.984806813297395,-0.188706783169536,
5.48852259094232));
#9266=CARTESIAN_POINT('Ctrl Pts',(0.984831692610592,-0.00389691057600537,
5.49834668730695));
#9267=CARTESIAN_POINT('Origin',(1.,-2.44249065417534E-15,5.425));
#9268=CARTESIAN_POINT('Origin',(1.,-2.44249065417534E-15,5.425));
#9269=CARTESIAN_POINT('Origin',(1.,0.,2.075));
#9270=CARTESIAN_POINT('',(0.,0.,0.));
#9271=CARTESIAN_POINT('Origin',(0.115470053837925,-1.,-0.2));
#9272=CARTESIAN_POINT('',(0.23094010767585,-1.,-1.11022302462516E-16));
#9273=CARTESIAN_POINT('',(0.115470053837925,-1.,-0.2));
#9274=CARTESIAN_POINT('',(0.23094010767585,-1.,-1.11022302462516E-16));
#9275=CARTESIAN_POINT('',(0.115470053837925,-1.3,-0.2));
#9276=CARTESIAN_POINT('',(0.115470053837925,-1.,-0.2));
#9277=CARTESIAN_POINT('',(0.23094010767585,-1.3,-1.11022302462516E-16));
#9278=CARTESIAN_POINT('',(0.23094010767585,-1.3,-1.11022302462516E-16));
#9279=CARTESIAN_POINT('',(0.23094010767585,-1.,-1.11022302462516E-16));
#9280=CARTESIAN_POINT('Origin',(-0.115470053837925,-1.,-0.2));
#9281=CARTESIAN_POINT('',(-0.115470053837925,-1.,-0.2));
#9282=CARTESIAN_POINT('',(0.115470053837925,-1.,-0.2));
#9283=CARTESIAN_POINT('',(-0.115470053837925,-1.3,-0.2));
#9284=CARTESIAN_POINT('',(-0.115470053837925,-1.,-0.2));
#9285=CARTESIAN_POINT('',(0.115470053837925,-1.3,-0.2));
#9286=CARTESIAN_POINT('Origin',(-0.23094010767585,-1.,-1.38777878078145E-16));
#9287=CARTESIAN_POINT('',(-0.23094010767585,-1.,-1.39304308828513E-16));
#9288=CARTESIAN_POINT('',(-0.115470053837925,-1.,-0.2));
#9289=CARTESIAN_POINT('',(-0.23094010767585,-1.3,-1.38777878078145E-16));
#9290=CARTESIAN_POINT('',(-0.23094010767585,-1.,-1.39304308828513E-16));
#9291=CARTESIAN_POINT('',(-0.115470053837925,-1.3,-0.2));
#9292=CARTESIAN_POINT('Origin',(-0.115470053837925,-1.,0.2));
#9293=CARTESIAN_POINT('',(-0.115470053837925,-1.,0.2));
#9294=CARTESIAN_POINT('',(-0.23094010767585,-1.,-1.39304308828513E-16));
#9295=CARTESIAN_POINT('',(-0.115470053837925,-1.3,0.2));
#9296=CARTESIAN_POINT('',(-0.115470053837925,-1.,0.2));
#9297=CARTESIAN_POINT('',(-0.23094010767585,-1.3,-1.39304308828513E-16));
#9298=CARTESIAN_POINT('Origin',(0.115470053837925,-1.,0.2));
#9299=CARTESIAN_POINT('',(0.115470053837925,-1.,0.2));
#9300=CARTESIAN_POINT('',(-0.115470053837925,-1.,0.2));
#9301=CARTESIAN_POINT('',(0.115470053837925,-1.3,0.2));
#9302=CARTESIAN_POINT('',(0.115470053837925,-1.,0.2));
#9303=CARTESIAN_POINT('',(-0.115470053837925,-1.3,0.2));
#9304=CARTESIAN_POINT('Origin',(0.23094010767585,-1.,-1.11022302462516E-16));
#9305=CARTESIAN_POINT('',(0.115470053837925,-1.,0.2));
#9306=CARTESIAN_POINT('',(0.115470053837925,-1.3,0.2));
#9307=CARTESIAN_POINT('Origin',(0.,-1.,-1.11022302462516E-16));
#9308=CARTESIAN_POINT('Origin',(0.,-1.3,-1.11022302462516E-16));
#9309=CARTESIAN_POINT('Origin',(0.,-1.9,-1.11022302462516E-16));
#9310=CARTESIAN_POINT('',(-0.24505,-1.9,-8.10123326494098E-17));
#9311=CARTESIAN_POINT('Origin',(0.,-1.9,-1.11022302462516E-16));
#9312=CARTESIAN_POINT('Origin',(0.375,0.,-1.11022302462516E-16));
#9313=CARTESIAN_POINT('',(-0.375,5.20417042793042E-17,-1.56946557430541E-16));
#9314=CARTESIAN_POINT('Origin',(0.,0.,-1.11022302462516E-16));
#9315=CARTESIAN_POINT('Origin',(0.,-0.0249999999999999,-1.11022302462516E-16));
#9316=CARTESIAN_POINT('',(-0.425,-0.0499999999999999,-1.63069791426278E-16));
#9317=CARTESIAN_POINT('Origin',(0.,-0.0499999999999998,-1.11022302462516E-16));
#9318=CARTESIAN_POINT('',(-0.4,-0.0249999999999999,-1.6000817442841E-16));
#9319=CARTESIAN_POINT('Origin',(0.,-0.26,-1.11022302462516E-16));
#9320=CARTESIAN_POINT('',(-0.425,-0.47,-1.63069791426278E-16));
#9321=CARTESIAN_POINT('Origin',(0.,-0.47,-1.11022302462516E-16));
#9322=CARTESIAN_POINT('',(-0.425,-0.26,-1.63069791426278E-16));
#9323=CARTESIAN_POINT('Origin',(0.,-0.485,-1.11022302462516E-16));
#9324=CARTESIAN_POINT('',(-0.395,-0.5,-1.59395851028836E-16));
#9325=CARTESIAN_POINT('Origin',(0.,-0.5,-1.11022302462516E-16));
#9326=CARTESIAN_POINT('',(-0.41,-0.485,-1.61232821227557E-16));
#9327=CARTESIAN_POINT('Origin',(0.27,-0.5,-1.11022302462516E-16));
#9328=CARTESIAN_POINT('',(-0.27,-0.5,-1.44087766039494E-16));
#9329=CARTESIAN_POINT('Origin',(0.,-0.5,-1.11022302462516E-16));
#9330=CARTESIAN_POINT('Origin',(0.,-0.52,-1.11022302462516E-16));
#9331=CARTESIAN_POINT('',(-0.24505,-0.5499,-8.10123326494098E-17));
#9332=CARTESIAN_POINT('Origin',(0.,-0.5499,-1.11022302462516E-16));
#9333=CARTESIAN_POINT('',(-0.26,-0.52,-1.42863119240347E-16));
#9334=CARTESIAN_POINT('Origin',(0.,-1.495,-1.11022302462516E-16));
#9335=CARTESIAN_POINT('',(-0.24505,-1.495,-1.41032272275622E-16));
#9336=CARTESIAN_POINT('',(0.,0.,0.));
#9337=CARTESIAN_POINT('',(0.,0.,0.));
#9338=CARTESIAN_POINT('',(0.,0.,0.));
#9339=CARTESIAN_POINT('',(0.,0.,0.));
#9340=CARTESIAN_POINT('',(0.,0.,0.));
#9341=CARTESIAN_POINT('',(0.,0.,0.));
#9342=CARTESIAN_POINT('',(0.989949493661167,0.989949493661166,2.));
#9343=CARTESIAN_POINT('',(-0.989949493661166,0.989949493661167,2.));
#9344=CARTESIAN_POINT('',(-0.989949493661167,-0.989949493661166,2.));
#9345=CARTESIAN_POINT('',(0.989949493661166,-0.989949493661167,2.));
#9346=CARTESIAN_POINT('',(0.,0.,0.));
#9347=CARTESIAN_POINT('',(0.,0.,0.));
#9348=CARTESIAN_POINT('Origin',(-1.23743686707646,-1.23743686707646,8.2));
#9349=CARTESIAN_POINT('',(-1.40243686707646,-1.23743686707646,8.2));
#9350=CARTESIAN_POINT('Origin',(-1.23743686707646,-1.23743686707646,8.2));
#9351=CARTESIAN_POINT('',(-1.40243686707646,-1.23743686707646,9.));
#9352=CARTESIAN_POINT('',(-1.40243686707646,-1.23743686707646,8.2));
#9353=CARTESIAN_POINT('Origin',(-1.23743686707646,-1.23743686707646,9.));
#9354=CARTESIAN_POINT('Origin',(-1.23743686707646,-1.23743686707646,8.2));
#9355=CARTESIAN_POINT('Origin',(-1.23743686707646,1.23743686707646,8.2));
#9356=CARTESIAN_POINT('',(-1.40243686707646,1.23743686707646,8.2));
#9357=CARTESIAN_POINT('Origin',(-1.23743686707646,1.23743686707646,8.2));
#9358=CARTESIAN_POINT('',(-1.40243686707646,1.23743686707646,9.));
#9359=CARTESIAN_POINT('',(-1.40243686707646,1.23743686707646,8.2));
#9360=CARTESIAN_POINT('Origin',(-1.23743686707646,1.23743686707646,9.));
#9361=CARTESIAN_POINT('Origin',(-1.23743686707646,1.23743686707646,8.2));
#9362=CARTESIAN_POINT('Origin',(1.23743686707646,1.23743686707646,8.2));
#9363=CARTESIAN_POINT('',(1.07243686707646,1.23743686707646,8.2));
#9364=CARTESIAN_POINT('Origin',(1.23743686707646,1.23743686707646,8.2));
#9365=CARTESIAN_POINT('',(1.07243686707646,1.23743686707646,9.));
#9366=CARTESIAN_POINT('',(1.07243686707646,1.23743686707646,8.2));
#9367=CARTESIAN_POINT('Origin',(1.23743686707646,1.23743686707646,9.));
#9368=CARTESIAN_POINT('Origin',(1.23743686707646,1.23743686707646,8.2));
#9369=CARTESIAN_POINT('Origin',(1.23743686707646,-1.23743686707646,8.2));
#9370=CARTESIAN_POINT('',(1.07243686707646,-1.23743686707646,8.2));
#9371=CARTESIAN_POINT('Origin',(1.23743686707646,-1.23743686707646,8.2));
#9372=CARTESIAN_POINT('',(1.07243686707646,-1.23743686707646,9.));
#9373=CARTESIAN_POINT('',(1.07243686707646,-1.23743686707646,8.2));
#9374=CARTESIAN_POINT('Origin',(1.23743686707646,-1.23743686707646,9.));
#9375=CARTESIAN_POINT('Origin',(1.23743686707646,-1.23743686707646,8.2));
#9376=CARTESIAN_POINT('Origin',(-1.23743686707646,-1.23743686707646,5.9));
#9377=CARTESIAN_POINT('',(-1.40243686707646,-1.23743686707646,6.));
#9378=CARTESIAN_POINT('Origin',(-1.23743686707646,-1.23743686707646,6.));
#9379=CARTESIAN_POINT('',(-1.40243686707646,-1.23743686707646,6.8));
#9380=CARTESIAN_POINT('',(-1.40243686707646,-1.23743686707646,5.9));
#9381=CARTESIAN_POINT('Origin',(-1.23743686707646,-1.23743686707646,6.8));
#9382=CARTESIAN_POINT('Origin',(-1.23743686707646,-1.23743686707646,6.8));
#9383=CARTESIAN_POINT('Origin',(-1.23743686707646,1.23743686707646,5.9));
#9384=CARTESIAN_POINT('',(-1.40243686707646,1.23743686707646,6.));
#9385=CARTESIAN_POINT('Origin',(-1.23743686707646,1.23743686707646,6.));
#9386=CARTESIAN_POINT('',(-1.40243686707646,1.23743686707646,6.8));
#9387=CARTESIAN_POINT('',(-1.40243686707646,1.23743686707646,5.9));
#9388=CARTESIAN_POINT('Origin',(-1.23743686707646,1.23743686707646,6.8));
#9389=CARTESIAN_POINT('Origin',(-1.23743686707646,1.23743686707646,6.8));
#9390=CARTESIAN_POINT('Origin',(1.23743686707646,1.23743686707646,5.9));
#9391=CARTESIAN_POINT('',(1.07243686707646,1.23743686707646,6.));
#9392=CARTESIAN_POINT('Origin',(1.23743686707646,1.23743686707646,6.));
#9393=CARTESIAN_POINT('',(1.07243686707646,1.23743686707646,6.8));
#9394=CARTESIAN_POINT('',(1.07243686707646,1.23743686707646,5.9));
#9395=CARTESIAN_POINT('Origin',(1.23743686707646,1.23743686707646,6.8));
#9396=CARTESIAN_POINT('Origin',(1.23743686707646,1.23743686707646,6.8));
#9397=CARTESIAN_POINT('Origin',(1.23743686707646,-1.23743686707646,5.9));
#9398=CARTESIAN_POINT('',(1.07243686707646,-1.23743686707646,6.));
#9399=CARTESIAN_POINT('Origin',(1.23743686707646,-1.23743686707646,6.));
#9400=CARTESIAN_POINT('',(1.07243686707646,-1.23743686707646,6.8));
#9401=CARTESIAN_POINT('',(1.07243686707646,-1.23743686707646,5.9));
#9402=CARTESIAN_POINT('Origin',(1.23743686707646,-1.23743686707646,6.8));
#9403=CARTESIAN_POINT('Origin',(1.23743686707646,-1.23743686707646,6.8));
#9404=CARTESIAN_POINT('Origin',(12.,0.,6.9));
#9405=CARTESIAN_POINT('',(11.75,-3.06161699786838E-17,7.));
#9406=CARTESIAN_POINT('Origin',(12.,0.,7.));
#9407=CARTESIAN_POINT('',(11.75,-3.06161699786838E-17,7.9));
#9408=CARTESIAN_POINT('',(11.75,-3.06161699786838E-17,6.9));
#9409=CARTESIAN_POINT('Origin',(12.,0.,7.9));
#9410=CARTESIAN_POINT('Origin',(12.,0.,7.9));
#9411=CARTESIAN_POINT('Origin',(12.,0.,7.));
#9412=CARTESIAN_POINT('',(10.8510874706924,0.8,8.2));
#9413=CARTESIAN_POINT('',(10.8510874706924,0.8,7.));
#9414=CARTESIAN_POINT('',(10.8510874706924,0.8,7.));
#9415=CARTESIAN_POINT('',(10.8510874706924,-0.8,8.2));
#9416=CARTESIAN_POINT('Origin',(12.,0.,8.2));
#9417=CARTESIAN_POINT('',(10.8510874706924,-0.8,7.));
#9418=CARTESIAN_POINT('',(10.8510874706924,-0.8,7.));
#9419=CARTESIAN_POINT('Origin',(12.,0.,7.));
#9420=CARTESIAN_POINT('Origin',(6.,0.,7.));
#9421=CARTESIAN_POINT('',(2.04939015319192,-0.8,7.));
#9422=CARTESIAN_POINT('',(0.,-0.8,7.));
#9423=CARTESIAN_POINT('',(2.04939015319192,0.8,7.));
#9424=CARTESIAN_POINT('Origin',(0.,0.,7.));
#9425=CARTESIAN_POINT('',(12.,0.8,7.));
#9426=CARTESIAN_POINT('Origin',(0.,-0.8,7.));
#9427=CARTESIAN_POINT('',(2.04939015319192,-0.8,8.2));
#9428=CARTESIAN_POINT('',(0.,-0.8,8.2));
#9429=CARTESIAN_POINT('',(2.04939015319192,-0.8,6.));
#9430=CARTESIAN_POINT('Origin',(12.,0.8,7.));
#9431=CARTESIAN_POINT('',(2.04939015319192,0.8,8.2));
#9432=CARTESIAN_POINT('',(2.04939015319192,0.8,6.));
#9433=CARTESIAN_POINT('',(12.,0.8,8.2));
#9434=CARTESIAN_POINT('Origin',(6.,0.,8.2));
#9435=CARTESIAN_POINT('Origin',(0.,0.,8.2));
#9436=CARTESIAN_POINT('Origin',(0.,0.,6.));
#9437=CARTESIAN_POINT('',(-1.5,-1.83697019872103E-16,9.));
#9438=CARTESIAN_POINT('Origin',(0.,0.,9.));
#9439=CARTESIAN_POINT('',(-1.5,-1.83697019872103E-16,6.));
#9440=CARTESIAN_POINT('',(-1.5,-1.83697019872103E-16,6.));
#9441=CARTESIAN_POINT('Origin',(0.,0.,6.));
#9442=CARTESIAN_POINT('Origin',(0.,0.,6.));
#9443=CARTESIAN_POINT('',(-2.2,-2.69422295812418E-16,9.));
#9444=CARTESIAN_POINT('Origin',(0.,0.,9.));
#9445=CARTESIAN_POINT('',(-2.2,-2.69422295812418E-16,6.));
#9446=CARTESIAN_POINT('',(-2.2,-2.69422295812418E-16,6.));
#9447=CARTESIAN_POINT('Origin',(0.,0.,6.));
#9448=CARTESIAN_POINT('Origin',(0.,0.,9.));
#9449=CARTESIAN_POINT('Origin',(0.,0.,6.));
#9450=CARTESIAN_POINT('',(0.,0.,0.));
#9451=CARTESIAN_POINT('Origin',(0.,0.,6.95));
#9452=CARTESIAN_POINT('',(-1.02,-1.2491397351303E-16,8.05));
#9453=CARTESIAN_POINT('Origin',(0.,0.,8.05));
#9454=CARTESIAN_POINT('',(-1.02,-1.2491397351303E-16,6.95));
#9455=CARTESIAN_POINT('',(-1.02,-1.2491397351303E-16,6.95));
#9456=CARTESIAN_POINT('Origin',(0.,0.,6.95));
#9457=CARTESIAN_POINT('Origin',(0.,0.,6.95));
#9458=CARTESIAN_POINT('',(-1.49,-1.82472373072956E-16,8.05));
#9459=CARTESIAN_POINT('Origin',(0.,0.,8.05));
#9460=CARTESIAN_POINT('',(-1.49,-1.82472373072956E-16,6.95));
#9461=CARTESIAN_POINT('',(-1.49,-1.82472373072956E-16,6.95));
#9462=CARTESIAN_POINT('Origin',(0.,0.,6.95));
#9463=CARTESIAN_POINT('Origin',(0.,0.,8.05));
#9464=CARTESIAN_POINT('Origin',(0.,0.,6.95));
#9465=CARTESIAN_POINT('',(0.,0.,0.));
#9466=CARTESIAN_POINT('Origin',(0.,0.,6.95));
#9467=CARTESIAN_POINT('',(-0.505,-6.18446633569413E-17,8.05));
#9468=CARTESIAN_POINT('Origin',(0.,0.,8.05));
#9469=CARTESIAN_POINT('',(-0.505,-6.18446633569413E-17,6.95));
#9470=CARTESIAN_POINT('',(-0.505,-6.18446633569413E-17,6.95));
#9471=CARTESIAN_POINT('Origin',(0.,0.,6.95));
#9472=CARTESIAN_POINT('Origin',(0.,0.,6.95));
#9473=CARTESIAN_POINT('',(-0.7,-8.57252759403147E-17,8.05));
#9474=CARTESIAN_POINT('Origin',(0.,0.,8.05));
#9475=CARTESIAN_POINT('',(-0.7,-8.57252759403147E-17,6.95));
#9476=CARTESIAN_POINT('',(-0.7,-8.57252759403147E-17,6.95));
#9477=CARTESIAN_POINT('Origin',(0.,0.,6.95));
#9478=CARTESIAN_POINT('Origin',(0.,0.,8.05));
#9479=CARTESIAN_POINT('Origin',(0.,0.,6.95));
#9480=CARTESIAN_POINT('',(0.,0.,0.));
#9481=CARTESIAN_POINT('Origin',(-1.23743686707646,-1.23743686707646,5.4));
#9482=CARTESIAN_POINT('',(-1.61243686707646,-1.23743686707646,5.5));
#9483=CARTESIAN_POINT('Origin',(-1.23743686707646,-1.23743686707646,5.5));
#9484=CARTESIAN_POINT('',(-1.61243686707646,-1.23743686707646,5.8));
#9485=CARTESIAN_POINT('',(-1.61243686707646,-1.23743686707646,5.4));
#9486=CARTESIAN_POINT('Origin',(-1.23743686707646,-1.23743686707646,5.8));
#9487=CARTESIAN_POINT('Origin',(-1.23743686707646,-1.23743686707646,5.8));
#9488=CARTESIAN_POINT('',(-1.46243686707646,-1.23743686707646,5.8));
#9489=CARTESIAN_POINT('Origin',(-1.23743686707646,-1.23743686707646,5.8));
#9490=CARTESIAN_POINT('Origin',(-1.23743686707646,1.23743686707646,5.4));
#9491=CARTESIAN_POINT('',(-1.61243686707646,1.23743686707646,5.5));
#9492=CARTESIAN_POINT('Origin',(-1.23743686707646,1.23743686707646,5.5));
#9493=CARTESIAN_POINT('',(-1.61243686707646,1.23743686707646,5.8));
#9494=CARTESIAN_POINT('',(-1.61243686707646,1.23743686707646,5.4));
#9495=CARTESIAN_POINT('Origin',(-1.23743686707646,1.23743686707646,5.8));
#9496=CARTESIAN_POINT('Origin',(-1.23743686707646,1.23743686707646,5.8));
#9497=CARTESIAN_POINT('',(-1.46243686707646,1.23743686707646,5.8));
#9498=CARTESIAN_POINT('Origin',(-1.23743686707646,1.23743686707646,5.8));
#9499=CARTESIAN_POINT('Origin',(1.23743686707646,1.23743686707646,5.4));
#9500=CARTESIAN_POINT('',(0.862436867076458,1.23743686707646,5.5));
#9501=CARTESIAN_POINT('Origin',(1.23743686707646,1.23743686707646,5.5));
#9502=CARTESIAN_POINT('',(0.862436867076458,1.23743686707646,5.8));
#9503=CARTESIAN_POINT('',(0.862436867076458,1.23743686707646,5.4));
#9504=CARTESIAN_POINT('Origin',(1.23743686707646,1.23743686707646,5.8));
#9505=CARTESIAN_POINT('Origin',(1.23743686707646,1.23743686707646,5.8));
#9506=CARTESIAN_POINT('',(1.01243686707646,1.23743686707646,5.8));
#9507=CARTESIAN_POINT('Origin',(1.23743686707646,1.23743686707646,5.8));
#9508=CARTESIAN_POINT('Origin',(1.23743686707646,-1.23743686707646,5.4));
#9509=CARTESIAN_POINT('',(0.862436867076458,-1.23743686707646,5.5));
#9510=CARTESIAN_POINT('Origin',(1.23743686707646,-1.23743686707646,5.5));
#9511=CARTESIAN_POINT('',(0.862436867076458,-1.23743686707646,5.8));
#9512=CARTESIAN_POINT('',(0.862436867076458,-1.23743686707646,5.4));
#9513=CARTESIAN_POINT('Origin',(1.23743686707646,-1.23743686707646,5.8));
#9514=CARTESIAN_POINT('Origin',(1.23743686707646,-1.23743686707646,5.8));
#9515=CARTESIAN_POINT('',(1.01243686707646,-1.23743686707646,5.8));
#9516=CARTESIAN_POINT('Origin',(1.23743686707646,-1.23743686707646,5.8));
#9517=CARTESIAN_POINT('Origin',(-1.23743686707646,-1.23743686707646,5.4));
#9518=CARTESIAN_POINT('',(-1.46243686707646,-1.23743686707646,6.));
#9519=CARTESIAN_POINT('',(-1.46243686707646,-1.23743686707646,5.4));
#9520=CARTESIAN_POINT('Origin',(-1.23743686707646,-1.23743686707646,6.));
#9521=CARTESIAN_POINT('Origin',(-1.23743686707646,1.23743686707646,5.4));
#9522=CARTESIAN_POINT('',(-1.46243686707646,1.23743686707646,6.));
#9523=CARTESIAN_POINT('',(-1.46243686707646,1.23743686707646,5.4));
#9524=CARTESIAN_POINT('Origin',(-1.23743686707646,1.23743686707646,6.));
#9525=CARTESIAN_POINT('Origin',(1.23743686707646,1.23743686707646,5.4));
#9526=CARTESIAN_POINT('',(1.01243686707646,1.23743686707646,6.));
#9527=CARTESIAN_POINT('',(1.01243686707646,1.23743686707646,5.4));
#9528=CARTESIAN_POINT('Origin',(1.23743686707646,1.23743686707646,6.));
#9529=CARTESIAN_POINT('Origin',(1.23743686707646,-1.23743686707646,5.4));
#9530=CARTESIAN_POINT('',(1.01243686707646,-1.23743686707646,6.));
#9531=CARTESIAN_POINT('',(1.01243686707646,-1.23743686707646,5.4));
#9532=CARTESIAN_POINT('Origin',(1.23743686707646,-1.23743686707646,6.));
#9533=CARTESIAN_POINT('Origin',(0.,0.,6.));
#9534=CARTESIAN_POINT('',(-1.49,-1.82472373072956E-16,6.05));
#9535=CARTESIAN_POINT('Origin',(0.,0.,6.05));
#9536=CARTESIAN_POINT('',(-1.49,-1.82472373072956E-16,6.));
#9537=CARTESIAN_POINT('',(-1.49,-1.82472373072956E-16,6.));
#9538=CARTESIAN_POINT('Origin',(0.,0.,6.));
#9539=CARTESIAN_POINT('Origin',(0.,0.,6.05));
#9540=CARTESIAN_POINT('',(-0.71,-8.69499227394621E-17,6.05));
#9541=CARTESIAN_POINT('Origin',(0.,0.,6.05));
#9542=CARTESIAN_POINT('Origin',(0.,0.,5.5));
#9543=CARTESIAN_POINT('',(-0.71,-8.69499227394621E-17,5.5));
#9544=CARTESIAN_POINT('',(-0.71,-8.69499227394621E-17,5.5));
#9545=CARTESIAN_POINT('Origin',(0.,0.,5.5));
#9546=CARTESIAN_POINT('Origin',(0.,0.,5.5));
#9547=CARTESIAN_POINT('',(-2.2,-2.69422295812418E-16,6.));
#9548=CARTESIAN_POINT('Origin',(0.,0.,6.));
#9549=CARTESIAN_POINT('',(-2.2,-2.69422295812418E-16,5.5));
#9550=CARTESIAN_POINT('',(-2.2,-2.69422295812418E-16,5.5));
#9551=CARTESIAN_POINT('Origin',(0.,0.,5.5));
#9552=CARTESIAN_POINT('Origin',(0.,0.,6.));
#9553=CARTESIAN_POINT('Origin',(0.,0.,5.5));
#9554=CARTESIAN_POINT('',(0.,0.,0.));
#9555=CARTESIAN_POINT('Origin',(-1.23743686707646,-1.23743686707646,9.1));
#9556=CARTESIAN_POINT('',(-1.61243686707646,-1.23743686707646,9.1));
#9557=CARTESIAN_POINT('Origin',(-1.23743686707646,-1.23743686707646,9.1));
#9558=CARTESIAN_POINT('',(-1.61243686707646,-1.23743686707646,9.5));
#9559=CARTESIAN_POINT('',(-1.61243686707646,-1.23743686707646,9.1));
#9560=CARTESIAN_POINT('Origin',(-1.23743686707646,-1.23743686707646,9.5));
#9561=CARTESIAN_POINT('Origin',(-1.23743686707646,-1.23743686707646,9.1));
#9562=CARTESIAN_POINT('',(-1.46243686707646,-1.23743686707646,9.1));
#9563=CARTESIAN_POINT('Origin',(-1.23743686707646,-1.23743686707646,9.1));
#9564=CARTESIAN_POINT('Origin',(-1.23743686707646,1.23743686707646,9.1));
#9565=CARTESIAN_POINT('',(-1.61243686707646,1.23743686707646,9.1));
#9566=CARTESIAN_POINT('Origin',(-1.23743686707646,1.23743686707646,9.1));
#9567=CARTESIAN_POINT('',(-1.61243686707646,1.23743686707646,9.5));
#9568=CARTESIAN_POINT('',(-1.61243686707646,1.23743686707646,9.1));
#9569=CARTESIAN_POINT('Origin',(-1.23743686707646,1.23743686707646,9.5));
#9570=CARTESIAN_POINT('Origin',(-1.23743686707646,1.23743686707646,9.1));
#9571=CARTESIAN_POINT('',(-1.46243686707646,1.23743686707646,9.1));
#9572=CARTESIAN_POINT('Origin',(-1.23743686707646,1.23743686707646,9.1));
#9573=CARTESIAN_POINT('Origin',(1.23743686707646,1.23743686707646,9.1));
#9574=CARTESIAN_POINT('',(0.862436867076458,1.23743686707646,9.1));
#9575=CARTESIAN_POINT('Origin',(1.23743686707646,1.23743686707646,9.1));
#9576=CARTESIAN_POINT('',(0.862436867076458,1.23743686707646,9.5));
#9577=CARTESIAN_POINT('',(0.862436867076458,1.23743686707646,9.1));
#9578=CARTESIAN_POINT('Origin',(1.23743686707646,1.23743686707646,9.5));
#9579=CARTESIAN_POINT('Origin',(1.23743686707646,1.23743686707646,9.1));
#9580=CARTESIAN_POINT('',(1.01243686707646,1.23743686707646,9.1));
#9581=CARTESIAN_POINT('Origin',(1.23743686707646,1.23743686707646,9.1));
#9582=CARTESIAN_POINT('Origin',(1.23743686707646,-1.23743686707646,9.1));
#9583=CARTESIAN_POINT('',(0.862436867076458,-1.23743686707646,9.1));
#9584=CARTESIAN_POINT('Origin',(1.23743686707646,-1.23743686707646,9.1));
#9585=CARTESIAN_POINT('',(0.862436867076458,-1.23743686707646,9.5));
#9586=CARTESIAN_POINT('',(0.862436867076458,-1.23743686707646,9.1));
#9587=CARTESIAN_POINT('Origin',(1.23743686707646,-1.23743686707646,9.5));
#9588=CARTESIAN_POINT('Origin',(1.23743686707646,-1.23743686707646,9.1));
#9589=CARTESIAN_POINT('',(1.01243686707646,-1.23743686707646,9.1));
#9590=CARTESIAN_POINT('Origin',(1.23743686707646,-1.23743686707646,9.1));
#9591=CARTESIAN_POINT('Origin',(-1.23743686707646,-1.23743686707646,8.9));
#9592=CARTESIAN_POINT('',(-1.46243686707646,-1.23743686707646,9.));
#9593=CARTESIAN_POINT('Origin',(-1.23743686707646,-1.23743686707646,9.));
#9594=CARTESIAN_POINT('',(-1.46243686707646,-1.23743686707646,8.9));
#9595=CARTESIAN_POINT('Origin',(-1.23743686707646,1.23743686707646,8.9));
#9596=CARTESIAN_POINT('',(-1.46243686707646,1.23743686707646,9.));
#9597=CARTESIAN_POINT('Origin',(-1.23743686707646,1.23743686707646,9.));
#9598=CARTESIAN_POINT('',(-1.46243686707646,1.23743686707646,8.9));
#9599=CARTESIAN_POINT('Origin',(1.23743686707646,1.23743686707646,8.9));
#9600=CARTESIAN_POINT('',(1.01243686707646,1.23743686707646,9.));
#9601=CARTESIAN_POINT('Origin',(1.23743686707646,1.23743686707646,9.));
#9602=CARTESIAN_POINT('',(1.01243686707646,1.23743686707646,8.9));
#9603=CARTESIAN_POINT('Origin',(1.23743686707646,-1.23743686707646,8.9));
#9604=CARTESIAN_POINT('',(1.01243686707646,-1.23743686707646,9.));
#9605=CARTESIAN_POINT('Origin',(1.23743686707646,-1.23743686707646,9.));
#9606=CARTESIAN_POINT('',(1.01243686707646,-1.23743686707646,8.9));
#9607=CARTESIAN_POINT('Origin',(3.,0.8,9.));
#9608=CARTESIAN_POINT('',(2.04939015319192,0.8,9.5));
#9609=CARTESIAN_POINT('',(2.04939015319192,0.8,9.));
#9610=CARTESIAN_POINT('',(2.04939015319192,0.8,9.));
#9611=CARTESIAN_POINT('',(3.,0.8,9.5));
#9612=CARTESIAN_POINT('',(3.,0.8,9.5));
#9613=CARTESIAN_POINT('',(3.,0.8,9.));
#9614=CARTESIAN_POINT('',(3.,0.8,9.));
#9615=CARTESIAN_POINT('',(3.,0.8,9.));
#9616=CARTESIAN_POINT('Origin',(1.2,-0.8,9.));
#9617=CARTESIAN_POINT('',(2.04939015319192,-0.8,9.));
#9618=CARTESIAN_POINT('',(2.04939015319192,-0.8,9.5));
#9619=CARTESIAN_POINT('',(2.04939015319192,-0.8,9.));
#9620=CARTESIAN_POINT('',(3.,-0.8,9.));
#9621=CARTESIAN_POINT('',(1.2,-0.8,9.));
#9622=CARTESIAN_POINT('',(3.,-0.8,9.5));
#9623=CARTESIAN_POINT('',(3.,-0.8,9.));
#9624=CARTESIAN_POINT('',(1.2,-0.8,9.5));
#9625=CARTESIAN_POINT('Origin',(3.,-0.8,9.));
#9626=CARTESIAN_POINT('',(3.,-0.8,9.));
#9627=CARTESIAN_POINT('',(3.,-0.8,9.5));
#9628=CARTESIAN_POINT('Origin',(0.,0.,8.95));
#9629=CARTESIAN_POINT('',(-1.49,-1.82472373072956E-16,9.));
#9630=CARTESIAN_POINT('Origin',(0.,0.,9.));
#9631=CARTESIAN_POINT('',(-1.49,-1.82472373072956E-16,8.95));
#9632=CARTESIAN_POINT('',(-1.49,-1.82472373072956E-16,8.95));
#9633=CARTESIAN_POINT('Origin',(0.,0.,8.95));
#9634=CARTESIAN_POINT('Origin',(0.,0.,8.95));
#9635=CARTESIAN_POINT('',(-0.71,-8.69499227394621E-17,8.95));
#9636=CARTESIAN_POINT('Origin',(0.,0.,8.95));
#9637=CARTESIAN_POINT('Origin',(0.,0.,9.));
#9638=CARTESIAN_POINT('',(-0.71,-8.69499227394621E-17,9.5));
#9639=CARTESIAN_POINT('Origin',(0.,0.,9.5));
#9640=CARTESIAN_POINT('',(-0.71,-8.69499227394621E-17,9.));
#9641=CARTESIAN_POINT('Origin',(0.,0.,9.));
#9642=CARTESIAN_POINT('Origin',(0.,0.,9.));
#9643=CARTESIAN_POINT('Origin',(0.,0.,9.5));
#9644=CARTESIAN_POINT('Origin',(0.,0.,9.5));
#9645=CARTESIAN_POINT('Origin',(0.,0.,9.));
#9646=CARTESIAN_POINT('',(0.,0.,0.));
#9647=CARTESIAN_POINT('Origin',(12.,0.,7.));
#9648=CARTESIAN_POINT('',(11.7,-3.67394039744207E-17,7.8));
#9649=CARTESIAN_POINT('Origin',(12.,0.,7.8));
#9650=CARTESIAN_POINT('',(11.7,-3.67394039744207E-17,7.));
#9651=CARTESIAN_POINT('',(11.7,-3.67394039744207E-17,7.));
#9652=CARTESIAN_POINT('Origin',(12.,0.,7.));
#9653=CARTESIAN_POINT('Origin',(12.,0.,7.8));
#9654=CARTESIAN_POINT('Origin',(12.,0.,6.4));
#9655=CARTESIAN_POINT('',(10.8,-1.46957615897682E-16,7.));
#9656=CARTESIAN_POINT('Origin',(12.,0.,7.));
#9657=CARTESIAN_POINT('',(10.8,-1.46957615897682E-16,6.4));
#9658=CARTESIAN_POINT('',(10.8,-1.46957615897682E-16,6.4));
#9659=CARTESIAN_POINT('Origin',(12.,0.,6.4));
#9660=CARTESIAN_POINT('Origin',(12.,0.,7.));
#9661=CARTESIAN_POINT('Origin',(12.,0.,6.4));
#9662=CARTESIAN_POINT('',(0.,0.,0.));
#9663=CARTESIAN_POINT('Origin',(12.,0.,6.));
#9664=CARTESIAN_POINT('',(10.8,-1.46957615897682E-16,6.4));
#9665=CARTESIAN_POINT('Origin',(12.,0.,6.4));
#9666=CARTESIAN_POINT('',(10.8,-1.46957615897682E-16,6.));
#9667=CARTESIAN_POINT('',(10.8,-1.46957615897682E-16,6.));
#9668=CARTESIAN_POINT('Origin',(12.,0.,6.));
#9669=CARTESIAN_POINT('Origin',(12.,0.,6.4));
#9670=CARTESIAN_POINT('Origin',(12.,0.,6.));
#9671=CARTESIAN_POINT('',(0.,0.,0.));
#9672=CARTESIAN_POINT('',(0.,0.,0.));
#9673=CARTESIAN_POINT('Origin',(0.,0.,0.));
#9674=CARTESIAN_POINT('',(-0.976185,-0.246528389340863,-1.19548183562566E-16));
#9675=CARTESIAN_POINT('',(-1.19548183562566E-16,-0.246528389340863,0.976185));
#9676=CARTESIAN_POINT('Origin',(0.,-0.246528389340863,0.));
#9677=CARTESIAN_POINT('Origin',(0.,-0.246528389340863,0.));
#9678=CARTESIAN_POINT('',(-1.19548183562566E-16,0.246528389340863,0.976185));
#9679=CARTESIAN_POINT('Origin',(-1.22464679914735E-16,0.,1.));
#9680=CARTESIAN_POINT('',(-0.976185,0.246528389340863,1.19548183562566E-16));
#9681=CARTESIAN_POINT('Origin',(0.,0.246528389340863,0.));
#9682=CARTESIAN_POINT('Origin',(0.,0.246528389340863,0.));
#9683=CARTESIAN_POINT('Origin',(0.,0.,0.));
#9684=CARTESIAN_POINT('',(-0.976185,0.45,-1.19548183562566E-16));
#9685=CARTESIAN_POINT('',(-0.976185,0.,-1.19548183562566E-16));
#9686=CARTESIAN_POINT('Origin',(0.,0.45,0.));
#9687=CARTESIAN_POINT('Origin',(0.,0.,0.));
#9688=CARTESIAN_POINT('',(-0.5,-0.39,-6.12323399573677E-17));
#9689=CARTESIAN_POINT('Origin',(0.,-0.39,0.));
#9690=CARTESIAN_POINT('',(-0.5,0.39,-6.12323399573677E-17));
#9691=CARTESIAN_POINT('',(-0.5,0.,-6.12323399573677E-17));
#9692=CARTESIAN_POINT('Origin',(0.,0.39,0.));
#9693=CARTESIAN_POINT('Origin',(0.,0.42,0.));
#9694=CARTESIAN_POINT('',(-0.56,0.45,-6.85802207522518E-17));
#9695=CARTESIAN_POINT('',(-0.53,0.42,-6.49062803548097E-17));
#9696=CARTESIAN_POINT('Origin',(0.,0.45,0.));
#9697=CARTESIAN_POINT('Origin',(0.976185,0.45,0.));
#9698=CARTESIAN_POINT('Origin',(0.,0.,0.));
#9699=CARTESIAN_POINT('',(-0.976185,-0.45,-1.19548183562566E-16));
#9700=CARTESIAN_POINT('Origin',(0.,-0.45,0.));
#9701=CARTESIAN_POINT('',(-0.976185,0.,-1.19548183562566E-16));
#9702=CARTESIAN_POINT('Origin',(0.56,-0.45,0.));
#9703=CARTESIAN_POINT('',(-0.56,-0.45,-6.85802207522518E-17));
#9704=CARTESIAN_POINT('Origin',(0.,-0.45,0.));
#9705=CARTESIAN_POINT('Origin',(0.,-0.42,0.));
#9706=CARTESIAN_POINT('',(-0.53,-0.42,-6.49062803548097E-17));
#9707=CARTESIAN_POINT('',(0.,0.,0.));
#9708=CARTESIAN_POINT('Origin',(0.,0.,0.));
#9709=CARTESIAN_POINT('',(-1.023815,0.246528389340863,-1.25381176266905E-16));
#9710=CARTESIAN_POINT('',(-1.25381176266905E-16,0.246528389340863,1.023815));
#9711=CARTESIAN_POINT('Origin',(0.,0.246528389340863,0.));
#9712=CARTESIAN_POINT('Origin',(0.,0.246528389340863,0.));
#9713=CARTESIAN_POINT('',(-1.25381176266905E-16,-0.246528389340863,1.023815));
#9714=CARTESIAN_POINT('Origin',(-1.22464679914735E-16,0.,1.));
#9715=CARTESIAN_POINT('',(-1.023815,-0.246528389340863,1.25381176266905E-16));
#9716=CARTESIAN_POINT('Origin',(0.,-0.246528389340863,0.));
#9717=CARTESIAN_POINT('Origin',(0.,-0.246528389340863,0.));
#9718=CARTESIAN_POINT('Origin',(0.,0.,0.));
#9719=CARTESIAN_POINT('',(-1.023815,-0.45,-1.25381176266905E-16));
#9720=CARTESIAN_POINT('Origin',(0.,-0.45,0.));
#9721=CARTESIAN_POINT('',(-1.023815,0.,-1.25381176266905E-16));
#9722=CARTESIAN_POINT('Origin',(1.44,0.45,0.));
#9723=CARTESIAN_POINT('',(-1.44,0.45,-1.76349139077219E-16));
#9724=CARTESIAN_POINT('Origin',(0.,0.45,0.));
#9725=CARTESIAN_POINT('',(-1.023815,0.45,-1.25381176266905E-16));
#9726=CARTESIAN_POINT('Origin',(0.,0.45,0.));
#9727=CARTESIAN_POINT('Origin',(0.,0.42,0.));
#9728=CARTESIAN_POINT('',(-1.5,0.39,-1.83697019872103E-16));
#9729=CARTESIAN_POINT('Origin',(0.,0.39,0.));
#9730=CARTESIAN_POINT('',(-1.47,0.42,-1.80023079474661E-16));
#9731=CARTESIAN_POINT('Origin',(0.,0.,0.));
#9732=CARTESIAN_POINT('',(-1.5,-0.39,-1.83697019872103E-16));
#9733=CARTESIAN_POINT('Origin',(0.,-0.39,0.));
#9734=CARTESIAN_POINT('',(-1.5,0.,-1.83697019872103E-16));
#9735=CARTESIAN_POINT('Origin',(0.,-0.42,0.));
#9736=CARTESIAN_POINT('',(-1.44,-0.45,-1.76349139077219E-16));
#9737=CARTESIAN_POINT('Origin',(0.,-0.45,0.));
#9738=CARTESIAN_POINT('',(-1.47,-0.42,-1.80023079474661E-16));
#9739=CARTESIAN_POINT('Origin',(1.023815,-0.45,0.));
#9740=CARTESIAN_POINT('Origin',(0.,0.,0.));
#9741=CARTESIAN_POINT('',(-1.023815,0.,-1.25381176266905E-16));
#9742=CARTESIAN_POINT('',(0.,0.,0.));
#9743=CARTESIAN_POINT('Origin',(1.,0.,0.));
#9744=CARTESIAN_POINT('',(1.,-1.78583896120461E-33,0.23815));
#9745=CARTESIAN_POINT('',(1.,-1.78583896120461E-33,-0.23815));
#9746=CARTESIAN_POINT('Origin',(1.,0.,0.));
#9747=CARTESIAN_POINT('Origin',(0.707106781186548,0.,-0.707106781186547));
#9748=CARTESIAN_POINT('',(0.875504261126124,-1.78583896120461E-33,-0.538709301246971));
#9749=CARTESIAN_POINT('',(0.538709301246971,-1.78583896120461E-33,-0.875504261126124));
#9750=CARTESIAN_POINT('Origin',(0.707106781186548,0.,-0.707106781186547));
#9751=CARTESIAN_POINT('Origin',(6.12323399573677E-17,0.,-1.));
#9752=CARTESIAN_POINT('',(0.23815,-1.78583896120461E-33,-1.));
#9753=CARTESIAN_POINT('',(-0.23815,-1.78583896120461E-33,-1.));
#9754=CARTESIAN_POINT('Origin',(6.12323399573677E-17,0.,-1.));
#9755=CARTESIAN_POINT('Origin',(-0.707106781186547,0.,-0.707106781186548));
#9756=CARTESIAN_POINT('',(-0.538709301246971,-1.78583896120461E-33,-0.875504261126124));
#9757=CARTESIAN_POINT('',(-0.875504261126124,-1.78583896120461E-33,-0.538709301246971));
#9758=CARTESIAN_POINT('Origin',(-0.707106781186547,0.,-0.707106781186548));
#9759=CARTESIAN_POINT('Origin',(-1.,0.,-1.22464679914735E-16));
#9760=CARTESIAN_POINT('',(-1.,-1.78583896120461E-33,-0.23815));
#9761=CARTESIAN_POINT('',(-1.,-1.78583896120461E-33,0.23815));
#9762=CARTESIAN_POINT('Origin',(-1.,0.,-1.22464679914735E-16));
#9763=CARTESIAN_POINT('Origin',(-0.707106781186548,0.,0.707106781186547));
#9764=CARTESIAN_POINT('',(-0.875504261126124,-7.94881478324376E-33,0.538709301246971));
#9765=CARTESIAN_POINT('',(-0.538709301246971,4.37713686083455E-33,0.875504261126124));
#9766=CARTESIAN_POINT('Origin',(-0.707106781186548,0.,0.707106781186547));
#9767=CARTESIAN_POINT('Origin',(-1.83697019872103E-16,0.,1.));
#9768=CARTESIAN_POINT('',(-0.23815,-1.78583896120461E-33,1.));
#9769=CARTESIAN_POINT('',(0.23815,-1.78583896120461E-33,1.));
#9770=CARTESIAN_POINT('Origin',(-1.83697019872103E-16,0.,1.));
#9771=CARTESIAN_POINT('Origin',(0.707106781186547,0.,0.707106781186548));
#9772=CARTESIAN_POINT('',(0.538709301246971,-4.86732687222419E-33,0.875504261126124));
#9773=CARTESIAN_POINT('',(0.875504261126124,1.29564894981497E-33,0.538709301246971));
#9774=CARTESIAN_POINT('Origin',(0.707106781186547,0.,0.707106781186548));
#9775=CARTESIAN_POINT('',(0.,0.,0.));
#9776=CARTESIAN_POINT('Origin',(0.707106781186547,0.,0.707106781186548));
#9777=CARTESIAN_POINT('',(0.504455939115715,-0.04763,0.841298510752802));
#9778=CARTESIAN_POINT('',(0.841298510752802,-0.04763,0.504455939115715));
#9779=CARTESIAN_POINT('Ctrl Pts',(0.504455939115715,-0.04763,0.841298510752802));
#9780=CARTESIAN_POINT('Ctrl Pts',(0.508899795931835,-0.0740444353928835,
0.838633903678357));
#9781=CARTESIAN_POINT('Ctrl Pts',(0.517157748491652,-0.0999305678883309,
0.833661031856294));
#9782=CARTESIAN_POINT('Ctrl Pts',(0.537715343527944,-0.142345102874864,
0.820511285096538));
#9783=CARTESIAN_POINT('Ctrl Pts',(0.548874290046456,-0.159766064500479,
0.813159949759));
#9784=CARTESIAN_POINT('Ctrl Pts',(0.573915184558107,-0.190326085855194,
0.795684265985089));
#9785=CARTESIAN_POINT('Ctrl Pts',(0.587792702767295,-0.203463743702801,
0.78555112003688));
#9786=CARTESIAN_POINT('Ctrl Pts',(0.615966552324775,-0.224161999508995,
0.763642258217233));
#9787=CARTESIAN_POINT('Ctrl Pts',(0.631684198665438,-0.232861760990032,
0.750785745543687));
#9788=CARTESIAN_POINT('Ctrl Pts',(0.663382628119203,-0.244251601209411,
0.722929908501543));
#9789=CARTESIAN_POINT('Ctrl Pts',(0.679352081686668,-0.246942143572133,
0.707917883896095));
#9790=CARTESIAN_POINT('Ctrl Pts',(0.707917883896095,-0.246942143572133,
0.679352081686668));
#9791=CARTESIAN_POINT('Ctrl Pts',(0.722929908501543,-0.244251601209411,
0.663382628119203));
#9792=CARTESIAN_POINT('Ctrl Pts',(0.750785745543687,-0.232861760990032,
0.631684198665439));
#9793=CARTESIAN_POINT('Ctrl Pts',(0.763642258217232,-0.224161999508995,
0.615966552324775));
#9794=CARTESIAN_POINT('Ctrl Pts',(0.78555112003688,-0.203463743702801,0.587792702767295));
#9795=CARTESIAN_POINT('Ctrl Pts',(0.795684265985088,-0.190326085855194,
0.573915184558108));
#9796=CARTESIAN_POINT('Ctrl Pts',(0.813159949759,-0.15976606450048,0.548874290046456));
#9797=CARTESIAN_POINT('Ctrl Pts',(0.820511285096538,-0.142345102874864,
0.537715343527944));
#9798=CARTESIAN_POINT('Ctrl Pts',(0.833661031856294,-0.099930567888331,
0.517157748491653));
#9799=CARTESIAN_POINT('Ctrl Pts',(0.838633903678357,-0.0740444353928835,
0.508899795931835));
#9800=CARTESIAN_POINT('Ctrl Pts',(0.841298510752801,-0.0476299999999999,
0.504455939115715));
#9801=CARTESIAN_POINT('',(0.528110872004958,-0.04763,0.871530771444223));
#9802=CARTESIAN_POINT('Origin',(0.707106781186547,-0.04763,0.707106781186548));
#9803=CARTESIAN_POINT('',(0.871530771444223,-0.04763,0.528110872004959));
#9804=CARTESIAN_POINT('Ctrl Pts',(0.871530771444223,-0.0476300000000001,
0.528110872004958));
#9805=CARTESIAN_POINT('Ctrl Pts',(0.87014664509073,-0.0609922781173483,
0.530395067942936));
#9806=CARTESIAN_POINT('Ctrl Pts',(0.868149331745851,-0.0742967091364493,
0.533674141594226));
#9807=CARTESIAN_POINT('Ctrl Pts',(0.85981294420286,-0.115492077056649,0.54708917182331));
#9808=CARTESIAN_POINT('Ctrl Pts',(0.850993704737257,-0.141695629206859,
0.560922177770136));
#9809=CARTESIAN_POINT('Ctrl Pts',(0.830754510485543,-0.181890537957859,
0.590422647829571));
#9810=CARTESIAN_POINT('Ctrl Pts',(0.816896541396381,-0.201072148666545,
0.609616703125488));
#9811=CARTESIAN_POINT('Ctrl Pts',(0.792310597819928,-0.223955109275652,
0.641117951819998));
#9812=CARTESIAN_POINT('Ctrl Pts',(0.779109323683612,-0.232742381310829,
0.657208095763053));
#9813=CARTESIAN_POINT('Ctrl Pts',(0.750552691816206,-0.244234834628584,
0.68964083160521));
#9814=CARTESIAN_POINT('Ctrl Pts',(0.735185187071673,-0.246942143572133,
0.705971972091755));
#9815=CARTESIAN_POINT('Ctrl Pts',(0.705971972091754,-0.246942143572133,
0.735185187071673));
#9816=CARTESIAN_POINT('Ctrl Pts',(0.689640831605209,-0.244234834628584,
0.750552691816206));
#9817=CARTESIAN_POINT('Ctrl Pts',(0.657208095763052,-0.232742381310829,
0.779109323683612));
#9818=CARTESIAN_POINT('Ctrl Pts',(0.641117951819998,-0.223955109275652,
0.792310597819928));
#9819=CARTESIAN_POINT('Ctrl Pts',(0.609616703125487,-0.201072148666545,
0.816896541396382));
#9820=CARTESIAN_POINT('Ctrl Pts',(0.590422647829571,-0.181890537957858,
0.830754510485544));
#9821=CARTESIAN_POINT('Ctrl Pts',(0.560922177770135,-0.141695629206858,
0.850993704737257));
#9822=CARTESIAN_POINT('Ctrl Pts',(0.547089171823309,-0.115492077056649,
0.859812944202861));
#9823=CARTESIAN_POINT('Ctrl Pts',(0.533674141594226,-0.0742967091364491,
0.868149331745852));
#9824=CARTESIAN_POINT('Ctrl Pts',(0.530395067942936,-0.0609922781173483,
0.870146645090731));
#9825=CARTESIAN_POINT('Ctrl Pts',(0.528110872004958,-0.0476300000000001,
0.871530771444223));
#9826=CARTESIAN_POINT('Origin',(0.707106781186547,-0.04763,0.707106781186548));
#9827=CARTESIAN_POINT('Origin',(0.,-0.166705,0.));
#9828=CARTESIAN_POINT('',(0.242834539687906,-0.04763,0.989696097314));
#9829=CARTESIAN_POINT('Origin',(0.,-0.04763,0.));
#9830=CARTESIAN_POINT('',(-0.242834539687907,-0.04763,0.989696097314));
#9831=CARTESIAN_POINT('Ctrl Pts',(0.242834539687906,-0.04763,0.989696097314));
#9832=CARTESIAN_POINT('Ctrl Pts',(0.24024064412003,-0.0609922781173483,
0.990332542620729));
#9833=CARTESIAN_POINT('Ctrl Pts',(0.236509675094874,-0.0742967091364492,
0.991238884025248));
#9834=CARTESIAN_POINT('Ctrl Pts',(0.221129100087819,-0.115492077056649,
0.994830026707808));
#9835=CARTESIAN_POINT('Ctrl Pts',(0.205111543747588,-0.141695629206859,
0.998375294985966));
#9836=CARTESIAN_POINT('Ctrl Pts',(0.169940289819232,-0.181890537957859,
1.00492400591205));
#9837=CARTESIAN_POINT('Ctrl Pts',(0.1465689792446,-0.201072148666545,1.00869718865384));
#9838=CARTESIAN_POINT('Ctrl Pts',(0.106909345252087,-0.223955109275652,
1.01358704779679));
#9839=CARTESIAN_POINT('Ctrl Pts',(0.0861971848975941,-0.232742381310829,
1.0156297872271));
#9840=CARTESIAN_POINT('Ctrl Pts',(0.0430711894098822,-0.244234834628584,
1.01837060663223));
#9841=CARTESIAN_POINT('Ctrl Pts',(0.0206568624125605,-0.246942143572133,
1.019052));
#9842=CARTESIAN_POINT('Ctrl Pts',(-0.0206568624125608,-0.246942143572133,
1.019052));
#9843=CARTESIAN_POINT('Ctrl Pts',(-0.0430711894098825,-0.244234834628584,
1.01837060663223));
#9844=CARTESIAN_POINT('Ctrl Pts',(-0.0861971848975943,-0.232742381310829,
1.0156297872271));
#9845=CARTESIAN_POINT('Ctrl Pts',(-0.106909345252088,-0.223955109275652,
1.01358704779679));
#9846=CARTESIAN_POINT('Ctrl Pts',(-0.1465689792446,-0.201072148666545,1.00869718865384));
#9847=CARTESIAN_POINT('Ctrl Pts',(-0.169940289819232,-0.181890537957859,
1.00492400591205));
#9848=CARTESIAN_POINT('Ctrl Pts',(-0.205111543747588,-0.141695629206859,
0.998375294985966));
#9849=CARTESIAN_POINT('Ctrl Pts',(-0.221129100087819,-0.115492077056649,
0.994830026707808));
#9850=CARTESIAN_POINT('Ctrl Pts',(-0.236509675094875,-0.0742967091364493,
0.991238884025248));
#9851=CARTESIAN_POINT('Ctrl Pts',(-0.24024064412003,-0.0609922781173483,
0.990332542620729));
#9852=CARTESIAN_POINT('Ctrl Pts',(-0.242834539687907,-0.04763,0.989696097314));
#9853=CARTESIAN_POINT('',(-0.528110872004959,-0.04763,0.871530771444223));
#9854=CARTESIAN_POINT('Origin',(0.,-0.04763,0.));
#9855=CARTESIAN_POINT('',(-0.871530771444223,-0.04763,0.528110872004958));
#9856=CARTESIAN_POINT('Ctrl Pts',(-0.528110872004958,-0.0476300000000001,
0.871530771444223));
#9857=CARTESIAN_POINT('Ctrl Pts',(-0.530395067942936,-0.0609922781173484,
0.87014664509073));
#9858=CARTESIAN_POINT('Ctrl Pts',(-0.533674141594226,-0.0742967091364493,
0.868149331745851));
#9859=CARTESIAN_POINT('Ctrl Pts',(-0.54708917182331,-0.115492077056649,
0.85981294420286));
#9860=CARTESIAN_POINT('Ctrl Pts',(-0.560922177770136,-0.141695629206859,
0.850993704737257));
#9861=CARTESIAN_POINT('Ctrl Pts',(-0.590422647829571,-0.181890537957859,
0.830754510485543));
#9862=CARTESIAN_POINT('Ctrl Pts',(-0.609616703125488,-0.201072148666545,
0.816896541396381));
#9863=CARTESIAN_POINT('Ctrl Pts',(-0.641117951819998,-0.223955109275652,
0.792310597819928));
#9864=CARTESIAN_POINT('Ctrl Pts',(-0.657208095763053,-0.232742381310829,
0.779109323683611));
#9865=CARTESIAN_POINT('Ctrl Pts',(-0.68964083160521,-0.244234834628584,
0.750552691816205));
#9866=CARTESIAN_POINT('Ctrl Pts',(-0.705971972091755,-0.246942143572133,
0.735185187071673));
#9867=CARTESIAN_POINT('Ctrl Pts',(-0.735185187071673,-0.246942143572133,
0.705971972091754));
#9868=CARTESIAN_POINT('Ctrl Pts',(-0.750552691816206,-0.244234834628584,
0.689640831605209));
#9869=CARTESIAN_POINT('Ctrl Pts',(-0.779109323683612,-0.232742381310829,
0.657208095763052));
#9870=CARTESIAN_POINT('Ctrl Pts',(-0.792310597819928,-0.223955109275652,
0.641117951819998));
#9871=CARTESIAN_POINT('Ctrl Pts',(-0.816896541396382,-0.201072148666545,
0.609616703125487));
#9872=CARTESIAN_POINT('Ctrl Pts',(-0.830754510485544,-0.181890537957858,
0.590422647829571));
#9873=CARTESIAN_POINT('Ctrl Pts',(-0.850993704737257,-0.141695629206858,
0.560922177770135));
#9874=CARTESIAN_POINT('Ctrl Pts',(-0.859812944202861,-0.115492077056649,
0.547089171823309));
#9875=CARTESIAN_POINT('Ctrl Pts',(-0.868149331745852,-0.0742967091364491,
0.533674141594226));
#9876=CARTESIAN_POINT('Ctrl Pts',(-0.870146645090731,-0.0609922781173483,
0.530395067942936));
#9877=CARTESIAN_POINT('Ctrl Pts',(-0.871530771444223,-0.04763,0.528110872004958));
#9878=CARTESIAN_POINT('',(-0.989696097314,-0.04763,0.242834539687906));
#9879=CARTESIAN_POINT('Origin',(0.,-0.04763,0.));
#9880=CARTESIAN_POINT('',(-1.019052,-0.246942143572133,1.248489836334E-16));
#9881=CARTESIAN_POINT('Ctrl Pts',(-0.989696097314,-0.04763,0.242834539687906));
#9882=CARTESIAN_POINT('Ctrl Pts',(-0.990332542620729,-0.0609922781173483,
0.24024064412003));
#9883=CARTESIAN_POINT('Ctrl Pts',(-0.991238884025248,-0.0742967091364492,
0.236509675094874));
#9884=CARTESIAN_POINT('Ctrl Pts',(-0.994830026707808,-0.115492077056649,
0.221129100087819));
#9885=CARTESIAN_POINT('Ctrl Pts',(-0.998375294985966,-0.141695629206859,
0.205111543747588));
#9886=CARTESIAN_POINT('Ctrl Pts',(-1.00492400591205,-0.181890537957859,
0.169940289819232));
#9887=CARTESIAN_POINT('Ctrl Pts',(-1.00869718865384,-0.201072148666545,
0.1465689792446));
#9888=CARTESIAN_POINT('Ctrl Pts',(-1.01358704779679,-0.223955109275652,
0.106909345252088));
#9889=CARTESIAN_POINT('Ctrl Pts',(-1.0156297872271,-0.232742381310829,0.0861971848975944));
#9890=CARTESIAN_POINT('Ctrl Pts',(-1.01837060663223,-0.244234834628584,
0.0430711894098825));
#9891=CARTESIAN_POINT('Ctrl Pts',(-1.019052,-0.246942143572133,0.0206568624125608));
#9892=CARTESIAN_POINT('Ctrl Pts',(-1.019052,-0.246942143572133,1.2490009027033E-16));
#9893=CARTESIAN_POINT('',(-1.019052,-0.28578,1.24797876996471E-16));
#9894=CARTESIAN_POINT('',(-1.019052,-0.166705,1.24797876996471E-16));
#9895=CARTESIAN_POINT('Origin',(0.,-0.28578,0.));
#9896=CARTESIAN_POINT('',(-0.989696097314,-0.04763,-0.242834539687906));
#9897=CARTESIAN_POINT('Ctrl Pts',(-1.019052,-0.246942143572133,1.2490009027033E-16));
#9898=CARTESIAN_POINT('Ctrl Pts',(-1.019052,-0.246942143572133,-0.0206568624125605));
#9899=CARTESIAN_POINT('Ctrl Pts',(-1.01837060663223,-0.244234834628584,
-0.0430711894098822));
#9900=CARTESIAN_POINT('Ctrl Pts',(-1.0156297872271,-0.232742381310829,-0.0861971848975941));
#9901=CARTESIAN_POINT('Ctrl Pts',(-1.01358704779679,-0.223955109275652,
-0.106909345252087));
#9902=CARTESIAN_POINT('Ctrl Pts',(-1.00869718865384,-0.201072148666546,
-0.1465689792446));
#9903=CARTESIAN_POINT('Ctrl Pts',(-1.00492400591205,-0.181890537957859,
-0.169940289819232));
#9904=CARTESIAN_POINT('Ctrl Pts',(-0.998375294985966,-0.141695629206859,
-0.205111543747588));
#9905=CARTESIAN_POINT('Ctrl Pts',(-0.994830026707808,-0.11549207705665,
-0.221129100087819));
#9906=CARTESIAN_POINT('Ctrl Pts',(-0.991238884025248,-0.0742967091364495,
-0.236509675094874));
#9907=CARTESIAN_POINT('Ctrl Pts',(-0.990332542620729,-0.0609922781173484,
-0.24024064412003));
#9908=CARTESIAN_POINT('Ctrl Pts',(-0.989696097314,-0.0476300000000001,-0.242834539687907));
#9909=CARTESIAN_POINT('',(-0.871530771444223,-0.04763,-0.528110872004958));
#9910=CARTESIAN_POINT('Origin',(0.,-0.04763,0.));
#9911=CARTESIAN_POINT('',(-0.528110872004958,-0.04763,-0.871530771444223));
#9912=CARTESIAN_POINT('Ctrl Pts',(-0.871530771444223,-0.0476300000000001,
-0.528110872004958));
#9913=CARTESIAN_POINT('Ctrl Pts',(-0.87014664509073,-0.0609922781173484,
-0.530395067942936));
#9914=CARTESIAN_POINT('Ctrl Pts',(-0.868149331745851,-0.0742967091364494,
-0.533674141594226));
#9915=CARTESIAN_POINT('Ctrl Pts',(-0.85981294420286,-0.115492077056649,
-0.54708917182331));
#9916=CARTESIAN_POINT('Ctrl Pts',(-0.850993704737257,-0.141695629206859,
-0.560922177770136));
#9917=CARTESIAN_POINT('Ctrl Pts',(-0.830754510485543,-0.181890537957859,
-0.590422647829571));
#9918=CARTESIAN_POINT('Ctrl Pts',(-0.816896541396381,-0.201072148666546,
-0.609616703125488));
#9919=CARTESIAN_POINT('Ctrl Pts',(-0.792310597819928,-0.223955109275652,
-0.641117951819999));
#9920=CARTESIAN_POINT('Ctrl Pts',(-0.779109323683611,-0.232742381310829,
-0.657208095763053));
#9921=CARTESIAN_POINT('Ctrl Pts',(-0.750552691816205,-0.244234834628584,
-0.68964083160521));
#9922=CARTESIAN_POINT('Ctrl Pts',(-0.735185187071673,-0.246942143572133,
-0.705971972091755));
#9923=CARTESIAN_POINT('Ctrl Pts',(-0.705971972091754,-0.246942143572133,
-0.735185187071673));
#9924=CARTESIAN_POINT('Ctrl Pts',(-0.68964083160521,-0.244234834628584,
-0.750552691816206));
#9925=CARTESIAN_POINT('Ctrl Pts',(-0.657208095763052,-0.232742381310829,
-0.779109323683612));
#9926=CARTESIAN_POINT('Ctrl Pts',(-0.641117951819998,-0.223955109275652,
-0.792310597819928));
#9927=CARTESIAN_POINT('Ctrl Pts',(-0.609616703125488,-0.201072148666545,
-0.816896541396381));
#9928=CARTESIAN_POINT('Ctrl Pts',(-0.590422647829571,-0.181890537957859,
-0.830754510485543));
#9929=CARTESIAN_POINT('Ctrl Pts',(-0.560922177770136,-0.141695629206859,
-0.850993704737257));
#9930=CARTESIAN_POINT('Ctrl Pts',(-0.54708917182331,-0.115492077056649,
-0.85981294420286));
#9931=CARTESIAN_POINT('Ctrl Pts',(-0.533674141594226,-0.0742967091364494,
-0.868149331745852));
#9932=CARTESIAN_POINT('Ctrl Pts',(-0.530395067942936,-0.0609922781173484,
-0.870146645090731));
#9933=CARTESIAN_POINT('Ctrl Pts',(-0.528110872004958,-0.0476300000000001,
-0.871530771444223));
#9934=CARTESIAN_POINT('',(-0.242834539687906,-0.04763,-0.989696097314));
#9935=CARTESIAN_POINT('Origin',(0.,-0.04763,0.));
#9936=CARTESIAN_POINT('',(0.242834539687906,-0.04763,-0.989696097314));
#9937=CARTESIAN_POINT('Ctrl Pts',(-0.242834539687907,-0.04763,-0.989696097314));
#9938=CARTESIAN_POINT('Ctrl Pts',(-0.24024064412003,-0.0609922781173483,
-0.990332542620729));
#9939=CARTESIAN_POINT('Ctrl Pts',(-0.236509675094874,-0.0742967091364493,
-0.991238884025248));
#9940=CARTESIAN_POINT('Ctrl Pts',(-0.221129100087819,-0.115492077056649,
-0.994830026707808));
#9941=CARTESIAN_POINT('Ctrl Pts',(-0.205111543747588,-0.141695629206859,
-0.998375294985966));
#9942=CARTESIAN_POINT('Ctrl Pts',(-0.169940289819232,-0.181890537957859,
-1.00492400591205));
#9943=CARTESIAN_POINT('Ctrl Pts',(-0.1465689792446,-0.201072148666545,-1.00869718865384));
#9944=CARTESIAN_POINT('Ctrl Pts',(-0.106909345252087,-0.223955109275652,
-1.01358704779679));
#9945=CARTESIAN_POINT('Ctrl Pts',(-0.0861971848975942,-0.232742381310829,
-1.0156297872271));
#9946=CARTESIAN_POINT('Ctrl Pts',(-0.0430711894098823,-0.244234834628584,
-1.01837060663223));
#9947=CARTESIAN_POINT('Ctrl Pts',(-0.0206568624125606,-0.246942143572133,
-1.019052));
#9948=CARTESIAN_POINT('Ctrl Pts',(0.0206568624125607,-0.246942143572133,
-1.019052));
#9949=CARTESIAN_POINT('Ctrl Pts',(0.0430711894098824,-0.244234834628584,
-1.01837060663223));
#9950=CARTESIAN_POINT('Ctrl Pts',(0.0861971848975943,-0.232742381310829,
-1.0156297872271));
#9951=CARTESIAN_POINT('Ctrl Pts',(0.106909345252088,-0.223955109275652,
-1.01358704779679));
#9952=CARTESIAN_POINT('Ctrl Pts',(0.1465689792446,-0.201072148666545,-1.00869718865384));
#9953=CARTESIAN_POINT('Ctrl Pts',(0.169940289819232,-0.181890537957859,
-1.00492400591205));
#9954=CARTESIAN_POINT('Ctrl Pts',(0.205111543747588,-0.141695629206859,
-0.998375294985966));
#9955=CARTESIAN_POINT('Ctrl Pts',(0.221129100087819,-0.115492077056649,
-0.994830026707808));
#9956=CARTESIAN_POINT('Ctrl Pts',(0.236509675094874,-0.0742967091364493,
-0.991238884025248));
#9957=CARTESIAN_POINT('Ctrl Pts',(0.24024064412003,-0.0609922781173484,
-0.990332542620729));
#9958=CARTESIAN_POINT('Ctrl Pts',(0.242834539687907,-0.04763,-0.989696097314));
#9959=CARTESIAN_POINT('',(0.528110872004958,-0.04763,-0.871530771444223));
#9960=CARTESIAN_POINT('Origin',(0.,-0.04763,0.));
#9961=CARTESIAN_POINT('',(0.871530771444223,-0.04763,-0.528110872004958));
#9962=CARTESIAN_POINT('Ctrl Pts',(0.528110872004958,-0.0476300000000001,
-0.871530771444223));
#9963=CARTESIAN_POINT('Ctrl Pts',(0.530395067942936,-0.0609922781173484,
-0.870146645090731));
#9964=CARTESIAN_POINT('Ctrl Pts',(0.533674141594226,-0.0742967091364493,
-0.868149331745851));
#9965=CARTESIAN_POINT('Ctrl Pts',(0.54708917182331,-0.115492077056649,-0.85981294420286));
#9966=CARTESIAN_POINT('Ctrl Pts',(0.560922177770136,-0.141695629206859,
-0.850993704737257));
#9967=CARTESIAN_POINT('Ctrl Pts',(0.590422647829571,-0.181890537957859,
-0.830754510485543));
#9968=CARTESIAN_POINT('Ctrl Pts',(0.609616703125488,-0.201072148666545,
-0.816896541396381));
#9969=CARTESIAN_POINT('Ctrl Pts',(0.641117951819998,-0.223955109275652,
-0.792310597819928));
#9970=CARTESIAN_POINT('Ctrl Pts',(0.657208095763053,-0.232742381310829,
-0.779109323683612));
#9971=CARTESIAN_POINT('Ctrl Pts',(0.68964083160521,-0.244234834628584,-0.750552691816206));
#9972=CARTESIAN_POINT('Ctrl Pts',(0.705971972091755,-0.246942143572133,
-0.735185187071673));
#9973=CARTESIAN_POINT('Ctrl Pts',(0.735185187071673,-0.246942143572133,
-0.705971972091754));
#9974=CARTESIAN_POINT('Ctrl Pts',(0.750552691816206,-0.244234834628584,
-0.68964083160521));
#9975=CARTESIAN_POINT('Ctrl Pts',(0.779109323683612,-0.232742381310829,
-0.657208095763053));
#9976=CARTESIAN_POINT('Ctrl Pts',(0.792310597819928,-0.223955109275652,
-0.641117951819998));
#9977=CARTESIAN_POINT('Ctrl Pts',(0.816896541396381,-0.201072148666545,
-0.609616703125488));
#9978=CARTESIAN_POINT('Ctrl Pts',(0.830754510485543,-0.181890537957859,
-0.590422647829571));
#9979=CARTESIAN_POINT('Ctrl Pts',(0.850993704737257,-0.141695629206859,
-0.560922177770136));
#9980=CARTESIAN_POINT('Ctrl Pts',(0.85981294420286,-0.115492077056649,-0.54708917182331));
#9981=CARTESIAN_POINT('Ctrl Pts',(0.868149331745851,-0.0742967091364493,
-0.533674141594226));
#9982=CARTESIAN_POINT('Ctrl Pts',(0.870146645090731,-0.0609922781173484,
-0.530395067942936));
#9983=CARTESIAN_POINT('Ctrl Pts',(0.871530771444223,-0.0476300000000001,
-0.528110872004958));
#9984=CARTESIAN_POINT('',(0.989696097314,-0.04763,-0.242834539687906));
#9985=CARTESIAN_POINT('Origin',(0.,-0.04763,0.));
#9986=CARTESIAN_POINT('',(0.989696097314,-0.04763,0.242834539687906));
#9987=CARTESIAN_POINT('Ctrl Pts',(0.989696097314,-0.04763,-0.242834539687907));
#9988=CARTESIAN_POINT('Ctrl Pts',(0.990332542620729,-0.0609922781173483,
-0.24024064412003));
#9989=CARTESIAN_POINT('Ctrl Pts',(0.991238884025248,-0.0742967091364493,
-0.236509675094874));
#9990=CARTESIAN_POINT('Ctrl Pts',(0.994830026707808,-0.115492077056649,
-0.221129100087819));
#9991=CARTESIAN_POINT('Ctrl Pts',(0.998375294985966,-0.141695629206859,
-0.205111543747588));
#9992=CARTESIAN_POINT('Ctrl Pts',(1.00492400591205,-0.181890537957859,-0.169940289819232));
#9993=CARTESIAN_POINT('Ctrl Pts',(1.00869718865384,-0.201072148666545,-0.1465689792446));
#9994=CARTESIAN_POINT('Ctrl Pts',(1.01358704779679,-0.223955109275652,-0.106909345252087));
#9995=CARTESIAN_POINT('Ctrl Pts',(1.0156297872271,-0.232742381310829,-0.0861971848975942));
#9996=CARTESIAN_POINT('Ctrl Pts',(1.01837060663223,-0.244234834628584,-0.0430711894098823));
#9997=CARTESIAN_POINT('Ctrl Pts',(1.019052,-0.246942143572133,-0.0206568624125607));
#9998=CARTESIAN_POINT('Ctrl Pts',(1.019052,-0.246942143572133,0.0206568624125607));
#9999=CARTESIAN_POINT('Ctrl Pts',(1.01837060663223,-0.244234834628584,0.0430711894098823));
#10000=CARTESIAN_POINT('Ctrl Pts',(1.0156297872271,-0.232742381310829,0.0861971848975942));
#10001=CARTESIAN_POINT('Ctrl Pts',(1.01358704779679,-0.223955109275652,
0.106909345252087));
#10002=CARTESIAN_POINT('Ctrl Pts',(1.00869718865384,-0.201072148666545,
0.1465689792446));
#10003=CARTESIAN_POINT('Ctrl Pts',(1.00492400591205,-0.181890537957859,
0.169940289819232));
#10004=CARTESIAN_POINT('Ctrl Pts',(0.998375294985966,-0.141695629206859,
0.205111543747588));
#10005=CARTESIAN_POINT('Ctrl Pts',(0.994830026707808,-0.115492077056649,
0.221129100087819));
#10006=CARTESIAN_POINT('Ctrl Pts',(0.991238884025248,-0.0742967091364492,
0.236509675094874));
#10007=CARTESIAN_POINT('Ctrl Pts',(0.990332542620729,-0.0609922781173483,
0.24024064412003));
#10008=CARTESIAN_POINT('Ctrl Pts',(0.989696097314,-0.04763,0.242834539687907));
#10009=CARTESIAN_POINT('Origin',(0.,-0.04763,0.));
#10010=CARTESIAN_POINT('Origin',(0.,-0.04763,0.));
#10011=CARTESIAN_POINT('',(0.238183666596899,-0.04763,0.951592097314));
#10012=CARTESIAN_POINT('Origin',(0.,-0.04763,0.));
#10013=CARTESIAN_POINT('Origin',(-1.94289029309402E-16,-0.04763,1.));
#10014=CARTESIAN_POINT('Origin',(-1.94289029309402E-16,0.,1.));
#10015=CARTESIAN_POINT('',(-0.2381836665969,-0.04763,0.951592097314));
#10016=CARTESIAN_POINT('Ctrl Pts',(-0.238183666596899,-0.0476299999999999,
0.951592097314));
#10017=CARTESIAN_POINT('Ctrl Pts',(-0.233157223576062,-0.0740444353928835,
0.952850216871763));
#10018=CARTESIAN_POINT('Ctrl Pts',(-0.223801617934946,-0.0999305678883309,
0.955173119738174));
#10019=CARTESIAN_POINT('Ctrl Pts',(-0.199966927975188,-0.142345102874864,
0.960411259488514));
#10020=CARTESIAN_POINT('Ctrl Pts',(-0.1868781821531,-0.159766064500479,
0.963103647174702));
#10021=CARTESIAN_POINT('Ctrl Pts',(-0.15681442133453,-0.190326085855194,
0.968453058988463));
#10022=CARTESIAN_POINT('Ctrl Pts',(-0.139836317888043,-0.203463743702801,
0.971100730005489));
#10023=CARTESIAN_POINT('Ctrl Pts',(-0.104422493053067,-0.224161999508995,
0.975530745318961));
#10024=CARTESIAN_POINT('Ctrl Pts',(-0.0842175114474176,-0.232861760990032,
0.977553872336861));
#10025=CARTESIAN_POINT('Ctrl Pts',(-0.0421062857595701,-0.244251601209411,
0.980270995488453));
#10026=CARTESIAN_POINT('Ctrl Pts',(-0.0201990724523197,-0.246942143572133,
0.980948));
#10027=CARTESIAN_POINT('Ctrl Pts',(0.020199072452319,-0.246942143572133,
0.980948));
#10028=CARTESIAN_POINT('Ctrl Pts',(0.0421062857595694,-0.244251601209411,
0.980270995488454));
#10029=CARTESIAN_POINT('Ctrl Pts',(0.0842175114474169,-0.232861760990032,
0.977553872336861));
#10030=CARTESIAN_POINT('Ctrl Pts',(0.104422493053067,-0.224161999508995,
0.975530745318961));
#10031=CARTESIAN_POINT('Ctrl Pts',(0.139836317888042,-0.203463743702801,
0.971100730005489));
#10032=CARTESIAN_POINT('Ctrl Pts',(0.15681442133453,-0.190326085855194,
0.968453058988463));
#10033=CARTESIAN_POINT('Ctrl Pts',(0.1868781821531,-0.15976606450048,0.963103647174702));
#10034=CARTESIAN_POINT('Ctrl Pts',(0.199966927975188,-0.142345102874864,
0.960411259488514));
#10035=CARTESIAN_POINT('Ctrl Pts',(0.223801617934945,-0.0999305678883309,
0.955173119738174));
#10036=CARTESIAN_POINT('Ctrl Pts',(0.233157223576061,-0.0740444353928835,
0.952850216871763));
#10037=CARTESIAN_POINT('Ctrl Pts',(0.238183666596899,-0.0476299999999999,
0.951592097314));
#10038=CARTESIAN_POINT('Origin',(-1.94289029309402E-16,-0.04763,1.));
#10039=CARTESIAN_POINT('Origin',(0.,-0.04763,0.));
#10040=CARTESIAN_POINT('',(-0.504455939115715,-0.04763,0.841298510752802));
#10041=CARTESIAN_POINT('Origin',(0.,-0.04763,0.));
#10042=CARTESIAN_POINT('Origin',(-0.707106781186548,-0.04763,0.707106781186547));
#10043=CARTESIAN_POINT('Origin',(-0.707106781186548,0.,0.707106781186547));
#10044=CARTESIAN_POINT('',(-0.841298510752802,-0.04763,0.504455939115715));
#10045=CARTESIAN_POINT('Ctrl Pts',(-0.841298510752802,-0.04763,0.504455939115715));
#10046=CARTESIAN_POINT('Ctrl Pts',(-0.838633903678357,-0.0740444353928835,
0.508899795931835));
#10047=CARTESIAN_POINT('Ctrl Pts',(-0.833661031856294,-0.0999305678883309,
0.517157748491652));
#10048=CARTESIAN_POINT('Ctrl Pts',(-0.820511285096538,-0.142345102874864,
0.537715343527944));
#10049=CARTESIAN_POINT('Ctrl Pts',(-0.813159949759,-0.159766064500479,0.548874290046456));
#10050=CARTESIAN_POINT('Ctrl Pts',(-0.795684265985089,-0.190326085855194,
0.573915184558107));
#10051=CARTESIAN_POINT('Ctrl Pts',(-0.78555112003688,-0.203463743702801,
0.587792702767295));
#10052=CARTESIAN_POINT('Ctrl Pts',(-0.763642258217233,-0.224161999508995,
0.615966552324775));
#10053=CARTESIAN_POINT('Ctrl Pts',(-0.750785745543687,-0.232861760990032,
0.631684198665438));
#10054=CARTESIAN_POINT('Ctrl Pts',(-0.722929908501543,-0.244251601209411,
0.663382628119203));
#10055=CARTESIAN_POINT('Ctrl Pts',(-0.707917883896095,-0.246942143572133,
0.679352081686668));
#10056=CARTESIAN_POINT('Ctrl Pts',(-0.679352081686668,-0.246942143572133,
0.707917883896095));
#10057=CARTESIAN_POINT('Ctrl Pts',(-0.663382628119203,-0.244251601209411,
0.722929908501544));
#10058=CARTESIAN_POINT('Ctrl Pts',(-0.631684198665438,-0.232861760990031,
0.750785745543687));
#10059=CARTESIAN_POINT('Ctrl Pts',(-0.615966552324775,-0.224161999508995,
0.763642258217233));
#10060=CARTESIAN_POINT('Ctrl Pts',(-0.587792702767295,-0.203463743702801,
0.78555112003688));
#10061=CARTESIAN_POINT('Ctrl Pts',(-0.573915184558107,-0.190326085855194,
0.795684265985088));
#10062=CARTESIAN_POINT('Ctrl Pts',(-0.548874290046456,-0.159766064500479,
0.813159949759));
#10063=CARTESIAN_POINT('Ctrl Pts',(-0.537715343527944,-0.142345102874864,
0.820511285096538));
#10064=CARTESIAN_POINT('Ctrl Pts',(-0.517157748491652,-0.0999305678883309,
0.833661031856294));
#10065=CARTESIAN_POINT('Ctrl Pts',(-0.508899795931835,-0.0740444353928835,
0.838633903678357));
#10066=CARTESIAN_POINT('Ctrl Pts',(-0.504455939115716,-0.04763,0.841298510752801));
#10067=CARTESIAN_POINT('Origin',(-0.707106781186548,-0.04763,0.707106781186547));
#10068=CARTESIAN_POINT('Origin',(0.,-0.04763,0.));
#10069=CARTESIAN_POINT('',(-0.951592097314,-0.04763,0.238183666596899));
#10070=CARTESIAN_POINT('Origin',(0.,-0.04763,0.));
#10071=CARTESIAN_POINT('Origin',(-1.,-0.04763,-1.11022302462516E-16));
#10072=CARTESIAN_POINT('Origin',(-1.,0.,-1.11022302462516E-16));
#10073=CARTESIAN_POINT('',(-0.951592097314,-0.04763,-0.2381836665969));
#10074=CARTESIAN_POINT('',(-0.980948,-0.246942143572133,1.08514323328844E-18));
#10075=CARTESIAN_POINT('Ctrl Pts',(-0.951592097314,-0.04763,-0.238183666596899));
#10076=CARTESIAN_POINT('Ctrl Pts',(-0.952850216871763,-0.0740444353928835,
-0.233157223576062));
#10077=CARTESIAN_POINT('Ctrl Pts',(-0.955173119738174,-0.0999305678883309,
-0.223801617934946));
#10078=CARTESIAN_POINT('Ctrl Pts',(-0.960411259488514,-0.142345102874864,
-0.199966927975188));
#10079=CARTESIAN_POINT('Ctrl Pts',(-0.963103647174702,-0.159766064500479,
-0.1868781821531));
#10080=CARTESIAN_POINT('Ctrl Pts',(-0.968453058988463,-0.190326085855194,
-0.15681442133453));
#10081=CARTESIAN_POINT('Ctrl Pts',(-0.971100730005489,-0.203463743702801,
-0.139836317888043));
#10082=CARTESIAN_POINT('Ctrl Pts',(-0.975530745318961,-0.224161999508995,
-0.104422493053067));
#10083=CARTESIAN_POINT('Ctrl Pts',(-0.977553872336861,-0.232861760990032,
-0.0842175114474175));
#10084=CARTESIAN_POINT('Ctrl Pts',(-0.980270995488453,-0.244251601209411,
-0.0421062857595699));
#10085=CARTESIAN_POINT('Ctrl Pts',(-0.980948,-0.246942143572133,-0.0201990724523195));
#10086=CARTESIAN_POINT('Ctrl Pts',(-0.980948,-0.246942143572133,-1.17961196366423E-16));
#10087=CARTESIAN_POINT('Origin',(-1.,-0.04763,-1.11022302462516E-16));
#10088=CARTESIAN_POINT('Ctrl Pts',(-0.980948,-0.246942143572133,-1.17961196366423E-16));
#10089=CARTESIAN_POINT('Ctrl Pts',(-0.980948,-0.246942143572133,0.0201990724523192));
#10090=CARTESIAN_POINT('Ctrl Pts',(-0.980270995488453,-0.244251601209411,
0.0421062857595695));
#10091=CARTESIAN_POINT('Ctrl Pts',(-0.977553872336861,-0.232861760990032,
0.0842175114474169));
#10092=CARTESIAN_POINT('Ctrl Pts',(-0.975530745318961,-0.224161999508995,
0.104422493053066));
#10093=CARTESIAN_POINT('Ctrl Pts',(-0.971100730005489,-0.203463743702801,
0.139836317888042));
#10094=CARTESIAN_POINT('Ctrl Pts',(-0.968453058988463,-0.190326085855194,
0.15681442133453));
#10095=CARTESIAN_POINT('Ctrl Pts',(-0.963103647174702,-0.15976606450048,
0.1868781821531));
#10096=CARTESIAN_POINT('Ctrl Pts',(-0.960411259488514,-0.142345102874864,
0.199966927975188));
#10097=CARTESIAN_POINT('Ctrl Pts',(-0.955173119738174,-0.099930567888331,
0.223801617934945));
#10098=CARTESIAN_POINT('Ctrl Pts',(-0.952850216871763,-0.0740444353928835,
0.233157223576061));
#10099=CARTESIAN_POINT('Ctrl Pts',(-0.951592097314,-0.04763,0.238183666596899));
#10100=CARTESIAN_POINT('Origin',(0.,-0.04763,0.));
#10101=CARTESIAN_POINT('',(-0.841298510752802,-0.04763,-0.504455939115715));
#10102=CARTESIAN_POINT('Origin',(0.,-0.04763,0.));
#10103=CARTESIAN_POINT('Origin',(-0.707106781186547,-0.04763,-0.707106781186548));
#10104=CARTESIAN_POINT('Origin',(-0.707106781186547,0.,-0.707106781186548));
#10105=CARTESIAN_POINT('',(-0.504455939115715,-0.04763,-0.841298510752802));
#10106=CARTESIAN_POINT('Ctrl Pts',(-0.504455939115715,-0.04763,-0.841298510752802));
#10107=CARTESIAN_POINT('Ctrl Pts',(-0.508899795931835,-0.0740444353928835,
-0.838633903678357));
#10108=CARTESIAN_POINT('Ctrl Pts',(-0.517157748491652,-0.0999305678883309,
-0.833661031856294));
#10109=CARTESIAN_POINT('Ctrl Pts',(-0.537715343527944,-0.142345102874864,
-0.820511285096538));
#10110=CARTESIAN_POINT('Ctrl Pts',(-0.548874290046456,-0.159766064500479,
-0.813159949759));
#10111=CARTESIAN_POINT('Ctrl Pts',(-0.573915184558107,-0.190326085855194,
-0.795684265985089));
#10112=CARTESIAN_POINT('Ctrl Pts',(-0.587792702767295,-0.203463743702801,
-0.78555112003688));
#10113=CARTESIAN_POINT('Ctrl Pts',(-0.615966552324775,-0.224161999508995,
-0.763642258217233));
#10114=CARTESIAN_POINT('Ctrl Pts',(-0.631684198665438,-0.232861760990032,
-0.750785745543687));
#10115=CARTESIAN_POINT('Ctrl Pts',(-0.663382628119203,-0.244251601209411,
-0.722929908501543));
#10116=CARTESIAN_POINT('Ctrl Pts',(-0.679352081686668,-0.246942143572133,
-0.707917883896095));
#10117=CARTESIAN_POINT('Ctrl Pts',(-0.707917883896095,-0.246942143572133,
-0.679352081686668));
#10118=CARTESIAN_POINT('Ctrl Pts',(-0.722929908501543,-0.244251601209411,
-0.663382628119203));
#10119=CARTESIAN_POINT('Ctrl Pts',(-0.750785745543687,-0.232861760990032,
-0.631684198665439));
#10120=CARTESIAN_POINT('Ctrl Pts',(-0.763642258217232,-0.224161999508995,
-0.615966552324775));
#10121=CARTESIAN_POINT('Ctrl Pts',(-0.78555112003688,-0.203463743702801,
-0.587792702767295));
#10122=CARTESIAN_POINT('Ctrl Pts',(-0.795684265985088,-0.190326085855194,
-0.573915184558107));
#10123=CARTESIAN_POINT('Ctrl Pts',(-0.813159949759,-0.15976606450048,-0.548874290046456));
#10124=CARTESIAN_POINT('Ctrl Pts',(-0.820511285096538,-0.142345102874864,
-0.537715343527944));
#10125=CARTESIAN_POINT('Ctrl Pts',(-0.833661031856294,-0.0999305678883311,
-0.517157748491652));
#10126=CARTESIAN_POINT('Ctrl Pts',(-0.838633903678357,-0.0740444353928836,
-0.508899795931835));
#10127=CARTESIAN_POINT('Ctrl Pts',(-0.841298510752801,-0.04763,-0.504455939115715));
#10128=CARTESIAN_POINT('Origin',(-0.707106781186547,-0.04763,-0.707106781186548));
#10129=CARTESIAN_POINT('Origin',(0.,-0.04763,0.));
#10130=CARTESIAN_POINT('',(-0.238183666596899,-0.04763,-0.951592097314));
#10131=CARTESIAN_POINT('Origin',(0.,-0.04763,0.));
#10132=CARTESIAN_POINT('Origin',(5.55111512312578E-17,-0.04763,-1.));
#10133=CARTESIAN_POINT('Origin',(5.55111512312578E-17,0.,-1.));
#10134=CARTESIAN_POINT('',(0.238183666596899,-0.04763,-0.951592097314));
#10135=CARTESIAN_POINT('Ctrl Pts',(0.238183666596899,-0.04763,-0.951592097314));
#10136=CARTESIAN_POINT('Ctrl Pts',(0.233157223576062,-0.0740444353928835,
-0.952850216871763));
#10137=CARTESIAN_POINT('Ctrl Pts',(0.223801617934946,-0.099930567888331,
-0.955173119738174));
#10138=CARTESIAN_POINT('Ctrl Pts',(0.199966927975188,-0.142345102874864,
-0.960411259488514));
#10139=CARTESIAN_POINT('Ctrl Pts',(0.1868781821531,-0.15976606450048,-0.963103647174702));
#10140=CARTESIAN_POINT('Ctrl Pts',(0.15681442133453,-0.190326085855194,
-0.968453058988463));
#10141=CARTESIAN_POINT('Ctrl Pts',(0.139836317888042,-0.203463743702801,
-0.971100730005489));
#10142=CARTESIAN_POINT('Ctrl Pts',(0.104422493053067,-0.224161999508995,
-0.975530745318961));
#10143=CARTESIAN_POINT('Ctrl Pts',(0.0842175114474173,-0.232861760990032,
-0.977553872336861));
#10144=CARTESIAN_POINT('Ctrl Pts',(0.0421062857595698,-0.244251601209411,
-0.980270995488453));
#10145=CARTESIAN_POINT('Ctrl Pts',(0.0201990724523194,-0.246942143572133,
-0.980948));
#10146=CARTESIAN_POINT('Ctrl Pts',(-0.0201990724523193,-0.246942143572133,
-0.980948));
#10147=CARTESIAN_POINT('Ctrl Pts',(-0.0421062857595697,-0.244251601209411,
-0.980270995488453));
#10148=CARTESIAN_POINT('Ctrl Pts',(-0.0842175114474171,-0.232861760990032,
-0.977553872336861));
#10149=CARTESIAN_POINT('Ctrl Pts',(-0.104422493053067,-0.224161999508995,
-0.975530745318961));
#10150=CARTESIAN_POINT('Ctrl Pts',(-0.139836317888042,-0.203463743702801,
-0.971100730005489));
#10151=CARTESIAN_POINT('Ctrl Pts',(-0.15681442133453,-0.190326085855194,
-0.968453058988463));
#10152=CARTESIAN_POINT('Ctrl Pts',(-0.1868781821531,-0.15976606450048,-0.963103647174702));
#10153=CARTESIAN_POINT('Ctrl Pts',(-0.199966927975188,-0.142345102874864,
-0.960411259488514));
#10154=CARTESIAN_POINT('Ctrl Pts',(-0.223801617934945,-0.099930567888331,
-0.955173119738174));
#10155=CARTESIAN_POINT('Ctrl Pts',(-0.233157223576062,-0.0740444353928835,
-0.952850216871763));
#10156=CARTESIAN_POINT('Ctrl Pts',(-0.238183666596899,-0.0476299999999999,
-0.951592097314));
#10157=CARTESIAN_POINT('Origin',(5.55111512312578E-17,-0.04763,-1.));
#10158=CARTESIAN_POINT('Origin',(0.,-0.04763,0.));
#10159=CARTESIAN_POINT('',(0.504455939115715,-0.04763,-0.841298510752802));
#10160=CARTESIAN_POINT('Origin',(0.,-0.04763,0.));
#10161=CARTESIAN_POINT('Origin',(0.707106781186548,-0.04763,-0.707106781186547));
#10162=CARTESIAN_POINT('Origin',(0.707106781186548,0.,-0.707106781186547));
#10163=CARTESIAN_POINT('',(0.841298510752802,-0.04763,-0.504455939115715));
#10164=CARTESIAN_POINT('Ctrl Pts',(0.841298510752802,-0.04763,-0.504455939115715));
#10165=CARTESIAN_POINT('Ctrl Pts',(0.838633903678357,-0.0740444353928835,
-0.508899795931835));
#10166=CARTESIAN_POINT('Ctrl Pts',(0.833661031856294,-0.0999305678883309,
-0.517157748491652));
#10167=CARTESIAN_POINT('Ctrl Pts',(0.820511285096538,-0.142345102874864,
-0.537715343527944));
#10168=CARTESIAN_POINT('Ctrl Pts',(0.813159949759,-0.159766064500479,-0.548874290046456));
#10169=CARTESIAN_POINT('Ctrl Pts',(0.795684265985088,-0.190326085855194,
-0.573915184558107));
#10170=CARTESIAN_POINT('Ctrl Pts',(0.78555112003688,-0.203463743702801,
-0.587792702767295));
#10171=CARTESIAN_POINT('Ctrl Pts',(0.763642258217233,-0.224161999508995,
-0.615966552324775));
#10172=CARTESIAN_POINT('Ctrl Pts',(0.750785745543687,-0.232861760990032,
-0.631684198665438));
#10173=CARTESIAN_POINT('Ctrl Pts',(0.722929908501543,-0.244251601209411,
-0.663382628119203));
#10174=CARTESIAN_POINT('Ctrl Pts',(0.707917883896095,-0.246942143572133,
-0.679352081686668));
#10175=CARTESIAN_POINT('Ctrl Pts',(0.679352081686668,-0.246942143572133,
-0.707917883896095));
#10176=CARTESIAN_POINT('Ctrl Pts',(0.663382628119203,-0.244251601209411,
-0.722929908501543));
#10177=CARTESIAN_POINT('Ctrl Pts',(0.631684198665438,-0.232861760990032,
-0.750785745543687));
#10178=CARTESIAN_POINT('Ctrl Pts',(0.615966552324775,-0.224161999508995,
-0.763642258217232));
#10179=CARTESIAN_POINT('Ctrl Pts',(0.587792702767295,-0.203463743702801,
-0.78555112003688));
#10180=CARTESIAN_POINT('Ctrl Pts',(0.573915184558107,-0.190326085855194,
-0.795684265985088));
#10181=CARTESIAN_POINT('Ctrl Pts',(0.548874290046456,-0.159766064500479,
-0.813159949759));
#10182=CARTESIAN_POINT('Ctrl Pts',(0.537715343527944,-0.142345102874864,
-0.820511285096538));
#10183=CARTESIAN_POINT('Ctrl Pts',(0.517157748491652,-0.099930567888331,
-0.833661031856294));
#10184=CARTESIAN_POINT('Ctrl Pts',(0.508899795931835,-0.0740444353928835,
-0.838633903678357));
#10185=CARTESIAN_POINT('Ctrl Pts',(0.504455939115715,-0.04763,-0.841298510752801));
#10186=CARTESIAN_POINT('Origin',(0.707106781186548,-0.04763,-0.707106781186547));
#10187=CARTESIAN_POINT('Origin',(0.,-0.166705,0.));
#10188=CARTESIAN_POINT('',(-0.980948,-0.28578,1.20131482833E-16));
#10189=CARTESIAN_POINT('Origin',(0.,-0.28578,0.));
#10190=CARTESIAN_POINT('',(-0.980948,-0.166705,1.20131482833E-16));
#10191=CARTESIAN_POINT('',(0.951592097314,-0.04763,0.238183666596899));
#10192=CARTESIAN_POINT('Origin',(0.,-0.04763,0.));
#10193=CARTESIAN_POINT('',(0.951592097314,-0.04763,-0.238183666596899));
#10194=CARTESIAN_POINT('Ctrl Pts',(0.951592097314,-0.04763,0.238183666596899));
#10195=CARTESIAN_POINT('Ctrl Pts',(0.952850216871763,-0.0740444353928835,
0.233157223576062));
#10196=CARTESIAN_POINT('Ctrl Pts',(0.955173119738174,-0.099930567888331,
0.223801617934945));
#10197=CARTESIAN_POINT('Ctrl Pts',(0.960411259488514,-0.142345102874864,
0.199966927975188));
#10198=CARTESIAN_POINT('Ctrl Pts',(0.963103647174702,-0.15976606450048,
0.1868781821531));
#10199=CARTESIAN_POINT('Ctrl Pts',(0.968453058988463,-0.190326085855194,
0.15681442133453));
#10200=CARTESIAN_POINT('Ctrl Pts',(0.971100730005489,-0.203463743702801,
0.139836317888042));
#10201=CARTESIAN_POINT('Ctrl Pts',(0.975530745318961,-0.224161999508995,
0.104422493053067));
#10202=CARTESIAN_POINT('Ctrl Pts',(0.977553872336861,-0.232861760990032,
0.0842175114474172));
#10203=CARTESIAN_POINT('Ctrl Pts',(0.980270995488453,-0.244251601209411,
0.0421062857595697));
#10204=CARTESIAN_POINT('Ctrl Pts',(0.980948,-0.246942143572133,0.0201990724523194));
#10205=CARTESIAN_POINT('Ctrl Pts',(0.980948,-0.246942143572133,-0.0201990724523194));
#10206=CARTESIAN_POINT('Ctrl Pts',(0.980270995488453,-0.244251601209411,
-0.0421062857595697));
#10207=CARTESIAN_POINT('Ctrl Pts',(0.977553872336861,-0.232861760990032,
-0.0842175114474172));
#10208=CARTESIAN_POINT('Ctrl Pts',(0.975530745318961,-0.224161999508995,
-0.104422493053067));
#10209=CARTESIAN_POINT('Ctrl Pts',(0.971100730005489,-0.203463743702801,
-0.139836317888042));
#10210=CARTESIAN_POINT('Ctrl Pts',(0.968453058988463,-0.190326085855194,
-0.15681442133453));
#10211=CARTESIAN_POINT('Ctrl Pts',(0.963103647174702,-0.15976606450048,
-0.1868781821531));
#10212=CARTESIAN_POINT('Ctrl Pts',(0.960411259488514,-0.142345102874864,
-0.199966927975188));
#10213=CARTESIAN_POINT('Ctrl Pts',(0.955173119738174,-0.099930567888331,
-0.223801617934945));
#10214=CARTESIAN_POINT('Ctrl Pts',(0.952850216871763,-0.0740444353928835,
-0.233157223576062));
#10215=CARTESIAN_POINT('Ctrl Pts',(0.951592097314,-0.0476299999999999,-0.238183666596899));
#10216=CARTESIAN_POINT('Origin',(0.,-0.04763,0.));
#10217=CARTESIAN_POINT('Origin',(0.,-0.04763,0.));
#10218=CARTESIAN_POINT('Origin',(1.,-0.04763,0.));
#10219=CARTESIAN_POINT('Origin',(1.,0.,0.));
#10220=CARTESIAN_POINT('Origin',(1.,-0.04763,0.));
#10221=CARTESIAN_POINT('Origin',(0.,-0.28578,0.));
#10222=CARTESIAN_POINT('Origin',(0.,-0.04763,0.));
#10223=CARTESIAN_POINT('',(0.,0.,0.));
#10224=CARTESIAN_POINT('Origin',(1.013815,0.445,0.));
#10225=CARTESIAN_POINT('',(-1.013815,0.445,-1.24156529467757E-16));
#10226=CARTESIAN_POINT('Origin',(0.,0.445,0.));
#10227=CARTESIAN_POINT('',(-0.991185,0.445,-1.21385153761287E-16));
#10228=CARTESIAN_POINT('Origin',(0.,0.445,0.));
#10229=CARTESIAN_POINT('Origin',(0.,0.4075,0.));
#10230=CARTESIAN_POINT('',(-1.013815,0.37,-1.24156529467757E-16));
#10231=CARTESIAN_POINT('Origin',(0.,0.37,0.));
#10232=CARTESIAN_POINT('',(-1.013815,0.4075,-1.24156529467757E-16));
#10233=CARTESIAN_POINT('Origin',(0.991185,0.37,0.));
#10234=CARTESIAN_POINT('',(-0.991185,0.37,-1.21385153761287E-16));
#10235=CARTESIAN_POINT('Origin',(0.,0.37,0.));
#10236=CARTESIAN_POINT('Origin',(0.,0.4075,0.));
#10237=CARTESIAN_POINT('',(-0.991185,0.4075,-1.21385153761287E-16));
#10238=CARTESIAN_POINT('Origin',(1.013815,-0.37,0.));
#10239=CARTESIAN_POINT('',(-1.013815,-0.37,-1.24156529467757E-16));
#10240=CARTESIAN_POINT('Origin',(0.,-0.37,0.));
#10241=CARTESIAN_POINT('',(-0.991185,-0.37,-1.21385153761287E-16));
#10242=CARTESIAN_POINT('Origin',(0.,-0.37,0.));
#10243=CARTESIAN_POINT('Origin',(0.,-0.4075,0.));
#10244=CARTESIAN_POINT('',(-1.013815,-0.445,-1.24156529467757E-16));
#10245=CARTESIAN_POINT('Origin',(0.,-0.445,0.));
#10246=CARTESIAN_POINT('',(-1.013815,-0.4075,-1.24156529467757E-16));
#10247=CARTESIAN_POINT('Origin',(0.991185,-0.445,0.));
#10248=CARTESIAN_POINT('',(-0.991185,-0.445,-1.21385153761287E-16));
#10249=CARTESIAN_POINT('Origin',(0.,-0.445,0.));
#10250=CARTESIAN_POINT('Origin',(0.,-0.4075,0.));
#10251=CARTESIAN_POINT('',(-0.991185,-0.4075,-1.21385153761287E-16));
#10252=CARTESIAN_POINT('',(0.,0.,0.));
#10253=CARTESIAN_POINT('',(0.,0.,0.));
#10254=CARTESIAN_POINT('',(0.,0.,0.));
#10255=CARTESIAN_POINT('',(0.,0.,0.));
#10256=CARTESIAN_POINT('',(0.,0.,0.));
#10257=CARTESIAN_POINT('',(0.,0.,0.));
#10258=CARTESIAN_POINT('',(0.,0.,0.));
#10259=CARTESIAN_POINT('Origin',(2.,0.9,10.5));
#10260=CARTESIAN_POINT('',(1.835,0.9,10.5));
#10261=CARTESIAN_POINT('Origin',(2.,0.9,10.5));
#10262=CARTESIAN_POINT('',(1.835,1.8,10.5));
#10263=CARTESIAN_POINT('',(1.835,0.9,10.5));
#10264=CARTESIAN_POINT('Origin',(2.,1.8,10.5));
#10265=CARTESIAN_POINT('Origin',(2.,0.9,10.5));
#10266=CARTESIAN_POINT('Origin',(2.,-2.3,10.5));
#10267=CARTESIAN_POINT('',(1.835,-2.2,10.5));
#10268=CARTESIAN_POINT('Origin',(2.,-2.2,10.5));
#10269=CARTESIAN_POINT('',(1.835,-1.2,10.5));
#10270=CARTESIAN_POINT('',(1.835,-2.3,10.5));
#10271=CARTESIAN_POINT('Origin',(2.,-1.2,10.5));
#10272=CARTESIAN_POINT('Origin',(2.,-1.2,10.5));
#10273=CARTESIAN_POINT('Origin',(2.,0.7,10.5));
#10274=CARTESIAN_POINT('',(1.5,0.7,10.5));
#10275=CARTESIAN_POINT('Origin',(2.,0.7,10.5));
#10276=CARTESIAN_POINT('',(1.7,0.7,10.5));
#10277=CARTESIAN_POINT('Origin',(2.,0.7,10.5));
#10278=CARTESIAN_POINT('Origin',(2.,0.5,10.5));
#10279=CARTESIAN_POINT('',(1.5,0.5,10.5));
#10280=CARTESIAN_POINT('',(1.5,0.5,10.5));
#10281=CARTESIAN_POINT('Origin',(2.,0.5,10.5));
#10282=CARTESIAN_POINT('Origin',(2.,-0.7,10.5));
#10283=CARTESIAN_POINT('',(1.5,-0.7,10.5));
#10284=CARTESIAN_POINT('Origin',(2.,-0.7,10.5));
#10285=CARTESIAN_POINT('',(1.7,-0.7,10.5));
#10286=CARTESIAN_POINT('Origin',(2.,-0.7,10.5));
#10287=CARTESIAN_POINT('Origin',(2.,-0.7,10.5));
#10288=CARTESIAN_POINT('',(1.5,-0.5,10.5));
#10289=CARTESIAN_POINT('Origin',(2.,-0.5,10.5));
#10290=CARTESIAN_POINT('',(1.5,-0.7,10.5));
#10291=CARTESIAN_POINT('Origin',(2.,-2.2,10.5));
#10292=CARTESIAN_POINT('',(1.7,-2.2,10.5));
#10293=CARTESIAN_POINT('',(1.7,-2.2,10.5));
#10294=CARTESIAN_POINT('Origin',(2.,-2.2,10.5));
#10295=CARTESIAN_POINT('Origin',(2.,-2.2,10.5));
#10296=CARTESIAN_POINT('',(1.7,1.8,10.5));
#10297=CARTESIAN_POINT('Origin',(2.,1.8,10.5));
#10298=CARTESIAN_POINT('',(1.7,-2.2,10.5));
#10299=CARTESIAN_POINT('Origin',(2.,1.8,10.5));
#10300=CARTESIAN_POINT('Origin',(2.,-2.2,10.5));
#10301=CARTESIAN_POINT('Origin',(2.,-0.5,10.7));
#10302=CARTESIAN_POINT('',(0.8,0.5,10.7));
#10303=CARTESIAN_POINT('Origin',(2.,0.5,10.7));
#10304=CARTESIAN_POINT('',(0.8,-0.5,10.7));
#10305=CARTESIAN_POINT('',(0.8,-0.5,10.7));
#10306=CARTESIAN_POINT('Origin',(2.,-0.5,10.7));
#10307=CARTESIAN_POINT('Origin',(2.,0.5,10.7));
#10308=CARTESIAN_POINT('Origin',(2.,-0.5,10.7));
#10309=CARTESIAN_POINT('',(0.,0.,0.));
#10310=CARTESIAN_POINT('Origin',(8.5,-2.3,10.5));
#10311=CARTESIAN_POINT('',(8.275,-2.2,10.5));
#10312=CARTESIAN_POINT('Origin',(8.5,-2.2,10.5));
#10313=CARTESIAN_POINT('',(8.275,-1.6,10.5));
#10314=CARTESIAN_POINT('',(8.275,-2.3,10.5));
#10315=CARTESIAN_POINT('Origin',(8.5,-1.6,10.5));
#10316=CARTESIAN_POINT('Origin',(8.5,-2.2,10.5));
#10317=CARTESIAN_POINT('',(7.9255437353462,-1.6,10.1));
#10318=CARTESIAN_POINT('',(7.9255437353462,-2.2,10.1));
#10319=CARTESIAN_POINT('',(7.9255437353462,-2.2,10.1));
#10320=CARTESIAN_POINT('',(7.9255437353462,-1.6,10.9));
#10321=CARTESIAN_POINT('Origin',(8.5,-1.6,10.5));
#10322=CARTESIAN_POINT('',(7.9255437353462,-2.2,10.9));
#10323=CARTESIAN_POINT('',(7.9255437353462,-2.2,10.9));
#10324=CARTESIAN_POINT('Origin',(8.5,-2.2,10.5));
#10325=CARTESIAN_POINT('Origin',(2.,-2.2,10.5));
#10326=CARTESIAN_POINT('',(2.5744562646538,-2.2,10.9));
#10327=CARTESIAN_POINT('',(8.5,-2.2,10.9));
#10328=CARTESIAN_POINT('',(1.3,-2.2,10.5));
#10329=CARTESIAN_POINT('Origin',(2.,-2.2,10.5));
#10330=CARTESIAN_POINT('',(2.5744562646538,-2.2,10.1));
#10331=CARTESIAN_POINT('Origin',(2.,-2.2,10.5));
#10332=CARTESIAN_POINT('',(2.,-2.2,10.1));
#10333=CARTESIAN_POINT('',(1.7,-2.2,10.5));
#10334=CARTESIAN_POINT('Origin',(2.,-2.2,10.5));
#10335=CARTESIAN_POINT('Origin',(2.,-2.2,10.9));
#10336=CARTESIAN_POINT('',(2.5744562646538,-1.6,10.9));
#10337=CARTESIAN_POINT('',(8.5,-1.6,10.9));
#10338=CARTESIAN_POINT('',(2.5744562646538,-2.2,10.9));
#10339=CARTESIAN_POINT('Origin',(8.5,-2.2,10.1));
#10340=CARTESIAN_POINT('',(2.5744562646538,-1.6,10.1));
#10341=CARTESIAN_POINT('',(2.5744562646538,-2.2,10.1));
#10342=CARTESIAN_POINT('',(2.,-1.6,10.1));
#10343=CARTESIAN_POINT('Origin',(5.25,-1.6,10.5));
#10344=CARTESIAN_POINT('Origin',(2.,-1.6,10.5));
#10345=CARTESIAN_POINT('Origin',(2.,-2.2,10.5));
#10346=CARTESIAN_POINT('',(1.7,-1.4,10.5));
#10347=CARTESIAN_POINT('Origin',(2.,-1.4,10.5));
#10348=CARTESIAN_POINT('',(1.7,-2.2,10.5));
#10349=CARTESIAN_POINT('Origin',(2.,-2.2,10.5));
#10350=CARTESIAN_POINT('',(1.3,-1.4,10.5));
#10351=CARTESIAN_POINT('Origin',(2.,-1.4,10.5));
#10352=CARTESIAN_POINT('',(1.3,-2.2,10.5));
#10353=CARTESIAN_POINT('Origin',(2.,-1.4,10.5));
#10354=CARTESIAN_POINT('',(0.,0.,0.));
#10355=CARTESIAN_POINT('Origin',(8.5,-3.3,10.5));
#10356=CARTESIAN_POINT('',(8.335,-3.3,10.5));
#10357=CARTESIAN_POINT('Origin',(8.5,-3.3,10.5));
#10358=CARTESIAN_POINT('',(8.335,-2.2,10.5));
#10359=CARTESIAN_POINT('',(8.335,-3.3,10.5));
#10360=CARTESIAN_POINT('Origin',(8.5,-2.2,10.5));
#10361=CARTESIAN_POINT('Origin',(8.5,-3.3,10.5));
#10362=CARTESIAN_POINT('Origin',(8.5,-4.2,10.5));
#10363=CARTESIAN_POINT('',(7.9,-2.2,10.5));
#10364=CARTESIAN_POINT('Origin',(8.5,-2.2,10.5));
#10365=CARTESIAN_POINT('',(7.9,-4.2,10.5));
#10366=CARTESIAN_POINT('',(7.9,-4.2,10.5));
#10367=CARTESIAN_POINT('Origin',(8.5,-4.2,10.5));
#10368=CARTESIAN_POINT('Origin',(8.5,-2.2,10.5));
#10369=CARTESIAN_POINT('Origin',(8.5,-4.2,10.5));
#10370=CARTESIAN_POINT('',(0.,0.,0.));
#10371=CARTESIAN_POINT('Origin',(2.,-2.4,10.5));
#10372=CARTESIAN_POINT('',(1.775,-2.2,10.5));
#10373=CARTESIAN_POINT('Origin',(2.,-2.2,10.5));
#10374=CARTESIAN_POINT('',(1.775,-2.4,10.5));
#10375=CARTESIAN_POINT('',(1.775,-2.4,10.5));
#10376=CARTESIAN_POINT('Origin',(2.,-2.4,10.5));
#10377=CARTESIAN_POINT('Origin',(2.,-2.4,10.5));
#10378=CARTESIAN_POINT('',(1.4,-2.2,10.5));
#10379=CARTESIAN_POINT('Origin',(2.,-2.2,10.5));
#10380=CARTESIAN_POINT('',(1.4,-2.4,10.5));
#10381=CARTESIAN_POINT('',(1.4,-2.4,10.5));
#10382=CARTESIAN_POINT('Origin',(2.,-2.4,10.5));
#10383=CARTESIAN_POINT('Origin',(2.,-2.2,10.5));
#10384=CARTESIAN_POINT('Origin',(2.,-2.4,10.5));
#10385=CARTESIAN_POINT('',(0.,0.,0.));
#10386=CARTESIAN_POINT('Origin',(2.,1.8,10.5));
#10387=CARTESIAN_POINT('',(1.775,2.,10.5));
#10388=CARTESIAN_POINT('Origin',(2.,2.,10.5));
#10389=CARTESIAN_POINT('',(1.775,1.8,10.5));
#10390=CARTESIAN_POINT('',(1.775,1.8,10.5));
#10391=CARTESIAN_POINT('Origin',(2.,1.8,10.5));
#10392=CARTESIAN_POINT('Origin',(2.,1.8,10.5));
#10393=CARTESIAN_POINT('',(1.4,2.,10.5));
#10394=CARTESIAN_POINT('Origin',(2.,2.,10.5));
#10395=CARTESIAN_POINT('',(1.4,1.8,10.5));
#10396=CARTESIAN_POINT('',(1.4,1.8,10.5));
#10397=CARTESIAN_POINT('Origin',(2.,1.8,10.5));
#10398=CARTESIAN_POINT('Origin',(2.,2.,10.5));
#10399=CARTESIAN_POINT('Origin',(2.,1.8,10.5));
#10400=CARTESIAN_POINT('',(0.,0.,0.));
#10401=CARTESIAN_POINT('Origin',(0.3,0.4,0.));
#10402=CARTESIAN_POINT('',(-0.3,0.4,-3.67394039744206E-17));
#10403=CARTESIAN_POINT('Origin',(0.,0.4,0.));
#10404=CARTESIAN_POINT('Origin',(0.,0.375,0.));
#10405=CARTESIAN_POINT('',(-0.35,0.35,-4.28626379701573E-17));
#10406=CARTESIAN_POINT('Origin',(0.,0.35,0.));
#10407=CARTESIAN_POINT('',(-0.325,0.375,-3.9801020972289E-17));
#10408=CARTESIAN_POINT('Origin',(0.,0.19,0.));
#10409=CARTESIAN_POINT('',(-0.35,0.03,-4.28626379701574E-17));
#10410=CARTESIAN_POINT('Origin',(0.,0.03,0.));
#10411=CARTESIAN_POINT('',(-0.35,0.19,-4.28626379701574E-17));
#10412=CARTESIAN_POINT('Origin',(0.,0.0149999999999999,0.));
#10413=CARTESIAN_POINT('',(-0.32,-3.29597460435593E-17,-3.91886975727153E-17));
#10414=CARTESIAN_POINT('Origin',(0.,0.,0.));
#10415=CARTESIAN_POINT('',(-0.335,0.0149999999999999,-4.10256677714363E-17));
#10416=CARTESIAN_POINT('Origin',(0.22,0.,0.));
#10417=CARTESIAN_POINT('',(-0.22,-6.93889390390723E-18,-2.69422295812418E-17));
#10418=CARTESIAN_POINT('Origin',(0.,0.,0.));
#10419=CARTESIAN_POINT('Origin',(0.,-0.02,0.));
#10420=CARTESIAN_POINT('',(-0.1954,-0.0492,2.39295984553393E-17));
#10421=CARTESIAN_POINT('Origin',(0.,-0.0492,0.));
#10422=CARTESIAN_POINT('',(-0.21,-0.02,-2.57175827820944E-17));
#10423=CARTESIAN_POINT('Origin',(0.,-0.8,0.));
#10424=CARTESIAN_POINT('',(-0.1954,-1.5646,2.39295984553393E-17));
#10425=CARTESIAN_POINT('Origin',(0.,-1.5646,0.));
#10426=CARTESIAN_POINT('',(-0.1954,-0.8,-2.39295984553393E-17));
#10427=CARTESIAN_POINT('Origin',(0.,-1.58,0.));
#10428=CARTESIAN_POINT('',(-0.16,-1.6,-1.95943487863577E-17));
#10429=CARTESIAN_POINT('Origin',(0.,-1.6,0.));
#10430=CARTESIAN_POINT('',(-0.18,-1.58,-2.20436423846524E-17));
#10431=CARTESIAN_POINT('Origin',(0.,-1.6,0.));
#10432=CARTESIAN_POINT('Origin',(0.0866025403784439,-0.4,-0.15));
#10433=CARTESIAN_POINT('',(0.173205080756888,-0.4,0.));
#10434=CARTESIAN_POINT('',(0.0866025403784439,-0.4,-0.15));
#10435=CARTESIAN_POINT('',(0.173205080756888,-0.4,0.));
#10436=CARTESIAN_POINT('',(0.0866025403784439,-0.64,-0.15));
#10437=CARTESIAN_POINT('',(0.0866025403784439,-0.4,-0.15));
#10438=CARTESIAN_POINT('',(0.173205080756888,-0.64,0.));
#10439=CARTESIAN_POINT('',(0.173205080756888,-0.64,0.));
#10440=CARTESIAN_POINT('',(0.173205080756888,-0.4,0.));
#10441=CARTESIAN_POINT('Origin',(-0.0866025403784438,-0.4,-0.15));
#10442=CARTESIAN_POINT('',(-0.0866025403784438,-0.4,-0.15));
#10443=CARTESIAN_POINT('',(0.0866025403784439,-0.4,-0.15));
#10444=CARTESIAN_POINT('',(-0.0866025403784438,-0.64,-0.15));
#10445=CARTESIAN_POINT('',(-0.0866025403784438,-0.4,-0.15));
#10446=CARTESIAN_POINT('',(0.0866025403784439,-0.64,-0.15));
#10447=CARTESIAN_POINT('Origin',(-0.173205080756888,-0.4,-2.77555756156289E-17));
#10448=CARTESIAN_POINT('',(-0.173205080756888,-0.4,-2.12115047744981E-17));
#10449=CARTESIAN_POINT('',(-0.0866025403784438,-0.4,-0.15));
#10450=CARTESIAN_POINT('',(-0.173205080756888,-0.64,-2.77555756156289E-17));
#10451=CARTESIAN_POINT('',(-0.173205080756888,-0.4,-2.12115047744981E-17));
#10452=CARTESIAN_POINT('',(-0.0866025403784438,-0.64,-0.15));
#10453=CARTESIAN_POINT('Origin',(-0.0866025403784439,-0.4,0.15));
#10454=CARTESIAN_POINT('',(-0.0866025403784439,-0.4,0.15));
#10455=CARTESIAN_POINT('',(-0.173205080756888,-0.4,-2.12115047744981E-17));
#10456=CARTESIAN_POINT('',(-0.0866025403784439,-0.64,0.15));
#10457=CARTESIAN_POINT('',(-0.0866025403784439,-0.4,0.15));
#10458=CARTESIAN_POINT('',(-0.173205080756888,-0.64,-2.12115047744981E-17));
#10459=CARTESIAN_POINT('Origin',(0.0866025403784439,-0.4,0.15));
#10460=CARTESIAN_POINT('',(0.0866025403784439,-0.4,0.15));
#10461=CARTESIAN_POINT('',(-0.0866025403784439,-0.4,0.15));
#10462=CARTESIAN_POINT('',(0.0866025403784439,-0.64,0.15));
#10463=CARTESIAN_POINT('',(0.0866025403784439,-0.4,0.15));
#10464=CARTESIAN_POINT('',(-0.0866025403784439,-0.64,0.15));
#10465=CARTESIAN_POINT('Origin',(0.173205080756888,-0.4,0.));
#10466=CARTESIAN_POINT('',(0.0866025403784439,-0.4,0.15));
#10467=CARTESIAN_POINT('',(0.0866025403784439,-0.64,0.15));
#10468=CARTESIAN_POINT('Origin',(0.,-0.4,-2.77555756156289E-17));
#10469=CARTESIAN_POINT('Origin',(0.,-0.64,-2.77555756156289E-17));
#10470=CARTESIAN_POINT('',(0.,0.,0.));
#10471=CARTESIAN_POINT('Origin',(0.0866025403784439,-0.4,-0.15));
#10472=CARTESIAN_POINT('',(0.173205080756888,-0.4,0.));
#10473=CARTESIAN_POINT('',(0.0866025403784439,-0.4,-0.15));
#10474=CARTESIAN_POINT('',(0.173205080756888,-0.4,0.));
#10475=CARTESIAN_POINT('',(0.0866025403784439,-0.64,-0.15));
#10476=CARTESIAN_POINT('',(0.0866025403784439,-0.4,-0.15));
#10477=CARTESIAN_POINT('',(0.173205080756888,-0.64,0.));
#10478=CARTESIAN_POINT('',(0.173205080756888,-0.64,0.));
#10479=CARTESIAN_POINT('',(0.173205080756888,-0.4,0.));
#10480=CARTESIAN_POINT('Origin',(-0.0866025403784438,-0.4,-0.15));
#10481=CARTESIAN_POINT('',(-0.0866025403784438,-0.4,-0.15));
#10482=CARTESIAN_POINT('',(0.0866025403784439,-0.4,-0.15));
#10483=CARTESIAN_POINT('',(-0.0866025403784438,-0.64,-0.15));
#10484=CARTESIAN_POINT('',(-0.0866025403784438,-0.4,-0.15));
#10485=CARTESIAN_POINT('',(0.0866025403784439,-0.64,-0.15));
#10486=CARTESIAN_POINT('Origin',(-0.173205080756888,-0.4,-2.77555756156289E-17));
#10487=CARTESIAN_POINT('',(-0.173205080756888,-0.4,-2.12115047744981E-17));
#10488=CARTESIAN_POINT('',(-0.0866025403784438,-0.4,-0.15));
#10489=CARTESIAN_POINT('',(-0.173205080756888,-0.64,-2.77555756156289E-17));
#10490=CARTESIAN_POINT('',(-0.173205080756888,-0.4,-2.12115047744981E-17));
#10491=CARTESIAN_POINT('',(-0.0866025403784438,-0.64,-0.15));
#10492=CARTESIAN_POINT('Origin',(-0.0866025403784439,-0.4,0.15));
#10493=CARTESIAN_POINT('',(-0.0866025403784439,-0.4,0.15));
#10494=CARTESIAN_POINT('',(-0.173205080756888,-0.4,-2.12115047744981E-17));
#10495=CARTESIAN_POINT('',(-0.0866025403784439,-0.64,0.15));
#10496=CARTESIAN_POINT('',(-0.0866025403784439,-0.4,0.15));
#10497=CARTESIAN_POINT('',(-0.173205080756888,-0.64,-2.12115047744981E-17));
#10498=CARTESIAN_POINT('Origin',(0.0866025403784439,-0.4,0.15));
#10499=CARTESIAN_POINT('',(0.0866025403784439,-0.4,0.15));
#10500=CARTESIAN_POINT('',(-0.0866025403784439,-0.4,0.15));
#10501=CARTESIAN_POINT('',(0.0866025403784439,-0.64,0.15));
#10502=CARTESIAN_POINT('',(0.0866025403784439,-0.4,0.15));
#10503=CARTESIAN_POINT('',(-0.0866025403784439,-0.64,0.15));
#10504=CARTESIAN_POINT('Origin',(0.173205080756888,-0.4,0.));
#10505=CARTESIAN_POINT('',(0.0866025403784439,-0.4,0.15));
#10506=CARTESIAN_POINT('',(0.0866025403784439,-0.64,0.15));
#10507=CARTESIAN_POINT('Origin',(0.,-0.4,-2.77555756156289E-17));
#10508=CARTESIAN_POINT('Origin',(0.,-0.64,-2.77555756156289E-17));
#10509=CARTESIAN_POINT('Origin',(0.,-1.,0.));
#10510=CARTESIAN_POINT('',(-0.1954,-1.,2.39295984553393E-17));
#10511=CARTESIAN_POINT('Origin',(0.,-1.,0.));
#10512=CARTESIAN_POINT('Origin',(0.3,0.4,0.));
#10513=CARTESIAN_POINT('',(-0.3,0.4,-3.67394039744206E-17));
#10514=CARTESIAN_POINT('Origin',(0.,0.4,0.));
#10515=CARTESIAN_POINT('Origin',(0.,0.375,0.));
#10516=CARTESIAN_POINT('',(-0.35,0.35,-4.28626379701573E-17));
#10517=CARTESIAN_POINT('Origin',(0.,0.35,0.));
#10518=CARTESIAN_POINT('',(-0.325,0.375,-3.9801020972289E-17));
#10519=CARTESIAN_POINT('Origin',(0.,0.19,0.));
#10520=CARTESIAN_POINT('',(-0.35,0.03,-4.28626379701574E-17));
#10521=CARTESIAN_POINT('Origin',(0.,0.03,0.));
#10522=CARTESIAN_POINT('',(-0.35,0.19,-4.28626379701574E-17));
#10523=CARTESIAN_POINT('Origin',(0.,0.0149999999999999,0.));
#10524=CARTESIAN_POINT('',(-0.32,-3.29597460435593E-17,-3.91886975727153E-17));
#10525=CARTESIAN_POINT('Origin',(0.,0.,0.));
#10526=CARTESIAN_POINT('',(-0.335,0.0149999999999999,-4.10256677714363E-17));
#10527=CARTESIAN_POINT('Origin',(0.22,0.,0.));
#10528=CARTESIAN_POINT('',(-0.22,-6.93889390390723E-18,-2.69422295812418E-17));
#10529=CARTESIAN_POINT('Origin',(0.,0.,0.));
#10530=CARTESIAN_POINT('Origin',(0.,-0.02,0.));
#10531=CARTESIAN_POINT('',(-0.1954,-0.0492,2.39295984553393E-17));
#10532=CARTESIAN_POINT('Origin',(0.,-0.0492,0.));
#10533=CARTESIAN_POINT('',(-0.21,-0.02,-2.57175827820944E-17));
#10534=CARTESIAN_POINT('Origin',(0.,-0.8,0.));
#10535=CARTESIAN_POINT('',(-0.1954,-0.8,-2.39295984553393E-17));
#10536=CARTESIAN_POINT('',(0.,0.,0.));
#10537=CARTESIAN_POINT('',(0.,0.,0.));
#10538=CARTESIAN_POINT('',(0.,0.,0.));
#10539=CARTESIAN_POINT('',(0.,0.,0.));
#10540=CARTESIAN_POINT('',(0.,0.,0.));
#10541=CARTESIAN_POINT('',(0.,0.,0.));
#10542=CARTESIAN_POINT('',(0.,0.,0.));
#10543=CARTESIAN_POINT('',(0.,0.,6.5));
#10544=CARTESIAN_POINT('',(0.,0.,8.5));
#10545=CARTESIAN_POINT('',(1.23743686707646,1.23743686707646,5.8));
#10546=CARTESIAN_POINT('',(-1.23743686707646,1.23743686707646,5.8));
#10547=CARTESIAN_POINT('',(-1.23743686707646,-1.23743686707646,5.8));
#10548=CARTESIAN_POINT('',(1.23743686707646,-1.23743686707646,5.8));
#10549=CARTESIAN_POINT('',(1.23743686707646,1.23743686707646,9.1));
#10550=CARTESIAN_POINT('',(-1.23743686707646,1.23743686707646,9.1));
#10551=CARTESIAN_POINT('',(-1.23743686707646,-1.23743686707646,9.1));
#10552=CARTESIAN_POINT('',(1.23743686707646,-1.23743686707646,9.1));
#10553=CARTESIAN_POINT('',(0.,0.,0.));
#10554=CARTESIAN_POINT('',(0.,0.,0.));
#10555=CARTESIAN_POINT('',(0.,0.,0.));
#10556=CARTESIAN_POINT('',(0.,0.,0.));
#10557=CARTESIAN_POINT('',(0.,0.,0.));
#10558=CARTESIAN_POINT('',(8.5,-1.6,10.5));
#10559=CARTESIAN_POINT('',(2.,-2.4,10.5));
#10560=CARTESIAN_POINT('',(2.,2.,10.5));
#10561=CARTESIAN_POINT('',(0.,0.,0.));
#10562=CARTESIAN_POINT('',(0.,0.,0.));
#10563=CARTESIAN_POINT('',(0.,0.,0.));
#10564=UNCERTAINTY_MEASURE_WITH_UNIT(LENGTH_MEASURE(0.001),#10628,
'DISTANCE_ACCURACY_VALUE',
'Maximum model space distance between geometric entities at asserted c
onnectivities');
#10565=UNCERTAINTY_MEASURE_WITH_UNIT(LENGTH_MEASURE(0.001),#10628,
'DISTANCE_ACCURACY_VALUE',
'Maximum model space distance between geometric entities at asserted c
onnectivities');
#10566=UNCERTAINTY_MEASURE_WITH_UNIT(LENGTH_MEASURE(0.001),#10628,
'DISTANCE_ACCURACY_VALUE',
'Maximum model space distance between geometric entities at asserted c
onnectivities');
#10567=UNCERTAINTY_MEASURE_WITH_UNIT(LENGTH_MEASURE(0.001),#10628,
'DISTANCE_ACCURACY_VALUE',
'Maximum model space distance between geometric entities at asserted c
onnectivities');
#10568=UNCERTAINTY_MEASURE_WITH_UNIT(LENGTH_MEASURE(0.001),#10628,
'DISTANCE_ACCURACY_VALUE',
'Maximum model space distance between geometric entities at asserted c
onnectivities');
#10569=UNCERTAINTY_MEASURE_WITH_UNIT(LENGTH_MEASURE(0.001),#10628,
'DISTANCE_ACCURACY_VALUE',
'Maximum model space distance between geometric entities at asserted c
onnectivities');
#10570=UNCERTAINTY_MEASURE_WITH_UNIT(LENGTH_MEASURE(0.001),#10628,
'DISTANCE_ACCURACY_VALUE',
'Maximum model space distance between geometric entities at asserted c
onnectivities');
#10571=UNCERTAINTY_MEASURE_WITH_UNIT(LENGTH_MEASURE(0.001),#10628,
'DISTANCE_ACCURACY_VALUE',
'Maximum model space distance between geometric entities at asserted c
onnectivities');
#10572=UNCERTAINTY_MEASURE_WITH_UNIT(LENGTH_MEASURE(0.001),#10628,
'DISTANCE_ACCURACY_VALUE',
'Maximum model space distance between geometric entities at asserted c
onnectivities');
#10573=UNCERTAINTY_MEASURE_WITH_UNIT(LENGTH_MEASURE(0.001),#10628,
'DISTANCE_ACCURACY_VALUE',
'Maximum model space distance between geometric entities at asserted c
onnectivities');
#10574=UNCERTAINTY_MEASURE_WITH_UNIT(LENGTH_MEASURE(0.001),#10628,
'DISTANCE_ACCURACY_VALUE',
'Maximum model space distance between geometric entities at asserted c
onnectivities');
#10575=UNCERTAINTY_MEASURE_WITH_UNIT(LENGTH_MEASURE(0.001),#10628,
'DISTANCE_ACCURACY_VALUE',
'Maximum model space distance between geometric entities at asserted c
onnectivities');
#10576=UNCERTAINTY_MEASURE_WITH_UNIT(LENGTH_MEASURE(0.001),#10628,
'DISTANCE_ACCURACY_VALUE',
'Maximum model space distance between geometric entities at asserted c
onnectivities');
#10577=UNCERTAINTY_MEASURE_WITH_UNIT(LENGTH_MEASURE(0.001),#10628,
'DISTANCE_ACCURACY_VALUE',
'Maximum model space distance between geometric entities at asserted c
onnectivities');
#10578=UNCERTAINTY_MEASURE_WITH_UNIT(LENGTH_MEASURE(0.001),#10628,
'DISTANCE_ACCURACY_VALUE',
'Maximum model space distance between geometric entities at asserted c
onnectivities');
#10579=UNCERTAINTY_MEASURE_WITH_UNIT(LENGTH_MEASURE(0.001),#10628,
'DISTANCE_ACCURACY_VALUE',
'Maximum model space distance between geometric entities at asserted c
onnectivities');
#10580=UNCERTAINTY_MEASURE_WITH_UNIT(LENGTH_MEASURE(0.001),#10628,
'DISTANCE_ACCURACY_VALUE',
'Maximum model space distance between geometric entities at asserted c
onnectivities');
#10581=UNCERTAINTY_MEASURE_WITH_UNIT(LENGTH_MEASURE(0.001),#10628,
'DISTANCE_ACCURACY_VALUE',
'Maximum model space distance between geometric entities at asserted c
onnectivities');
#10582=UNCERTAINTY_MEASURE_WITH_UNIT(LENGTH_MEASURE(0.001),#10628,
'DISTANCE_ACCURACY_VALUE',
'Maximum model space distance between geometric entities at asserted c
onnectivities');
#10583=UNCERTAINTY_MEASURE_WITH_UNIT(LENGTH_MEASURE(0.001),#10628,
'DISTANCE_ACCURACY_VALUE',
'Maximum model space distance between geometric entities at asserted c
onnectivities');
#10584=UNCERTAINTY_MEASURE_WITH_UNIT(LENGTH_MEASURE(0.001),#10628,
'DISTANCE_ACCURACY_VALUE',
'Maximum model space distance between geometric entities at asserted c
onnectivities');
#10585=UNCERTAINTY_MEASURE_WITH_UNIT(LENGTH_MEASURE(0.001),#10628,
'DISTANCE_ACCURACY_VALUE',
'Maximum model space distance between geometric entities at asserted c
onnectivities');
#10586=UNCERTAINTY_MEASURE_WITH_UNIT(LENGTH_MEASURE(0.001),#10628,
'DISTANCE_ACCURACY_VALUE',
'Maximum model space distance between geometric entities at asserted c
onnectivities');
#10587=UNCERTAINTY_MEASURE_WITH_UNIT(LENGTH_MEASURE(0.001),#10628,
'DISTANCE_ACCURACY_VALUE',
'Maximum model space distance between geometric entities at asserted c
onnectivities');
#10588=UNCERTAINTY_MEASURE_WITH_UNIT(LENGTH_MEASURE(0.001),#10628,
'DISTANCE_ACCURACY_VALUE',
'Maximum model space distance between geometric entities at asserted c
onnectivities');
#10589=UNCERTAINTY_MEASURE_WITH_UNIT(LENGTH_MEASURE(0.001),#10628,
'DISTANCE_ACCURACY_VALUE',
'Maximum model space distance between geometric entities at asserted c
onnectivities');
#10590=UNCERTAINTY_MEASURE_WITH_UNIT(LENGTH_MEASURE(0.001),#10628,
'DISTANCE_ACCURACY_VALUE',
'Maximum model space distance between geometric entities at asserted c
onnectivities');
#10591=UNCERTAINTY_MEASURE_WITH_UNIT(LENGTH_MEASURE(0.001),#10628,
'DISTANCE_ACCURACY_VALUE',
'Maximum model space distance between geometric entities at asserted c
onnectivities');
#10592=UNCERTAINTY_MEASURE_WITH_UNIT(LENGTH_MEASURE(0.001),#10628,
'DISTANCE_ACCURACY_VALUE',
'Maximum model space distance between geometric entities at asserted c
onnectivities');
#10593=UNCERTAINTY_MEASURE_WITH_UNIT(LENGTH_MEASURE(0.001),#10628,
'DISTANCE_ACCURACY_VALUE',
'Maximum model space distance between geometric entities at asserted c
onnectivities');
#10594=UNCERTAINTY_MEASURE_WITH_UNIT(LENGTH_MEASURE(0.001),#10628,
'DISTANCE_ACCURACY_VALUE',
'Maximum model space distance between geometric entities at asserted c
onnectivities');
#10595=UNCERTAINTY_MEASURE_WITH_UNIT(LENGTH_MEASURE(0.001),#10628,
'DISTANCE_ACCURACY_VALUE',
'Maximum model space distance between geometric entities at asserted c
onnectivities');
#10596=(
GEOMETRIC_REPRESENTATION_CONTEXT(3)
GLOBAL_UNCERTAINTY_ASSIGNED_CONTEXT((#10564))
GLOBAL_UNIT_ASSIGNED_CONTEXT((#10628,#10630,#10631))
REPRESENTATION_CONTEXT('','3D')
);
#10597=(
GEOMETRIC_REPRESENTATION_CONTEXT(3)
GLOBAL_UNCERTAINTY_ASSIGNED_CONTEXT((#10565))
GLOBAL_UNIT_ASSIGNED_CONTEXT((#10628,#10630,#10631))
REPRESENTATION_CONTEXT('','3D')
);
#10598=(
GEOMETRIC_REPRESENTATION_CONTEXT(3)
GLOBAL_UNCERTAINTY_ASSIGNED_CONTEXT((#10566))
GLOBAL_UNIT_ASSIGNED_CONTEXT((#10628,#10630,#10631))
REPRESENTATION_CONTEXT('','3D')
);
#10599=(
GEOMETRIC_REPRESENTATION_CONTEXT(3)
GLOBAL_UNCERTAINTY_ASSIGNED_CONTEXT((#10567))
GLOBAL_UNIT_ASSIGNED_CONTEXT((#10628,#10630,#10631))
REPRESENTATION_CONTEXT('','3D')
);
#10600=(
GEOMETRIC_REPRESENTATION_CONTEXT(3)
GLOBAL_UNCERTAINTY_ASSIGNED_CONTEXT((#10568))
GLOBAL_UNIT_ASSIGNED_CONTEXT((#10628,#10630,#10631))
REPRESENTATION_CONTEXT('','3D')
);
#10601=(
GEOMETRIC_REPRESENTATION_CONTEXT(3)
GLOBAL_UNCERTAINTY_ASSIGNED_CONTEXT((#10569))
GLOBAL_UNIT_ASSIGNED_CONTEXT((#10628,#10630,#10631))
REPRESENTATION_CONTEXT('','3D')
);
#10602=(
GEOMETRIC_REPRESENTATION_CONTEXT(3)
GLOBAL_UNCERTAINTY_ASSIGNED_CONTEXT((#10570))
GLOBAL_UNIT_ASSIGNED_CONTEXT((#10628,#10630,#10631))
REPRESENTATION_CONTEXT('','3D')
);
#10603=(
GEOMETRIC_REPRESENTATION_CONTEXT(3)
GLOBAL_UNCERTAINTY_ASSIGNED_CONTEXT((#10571))
GLOBAL_UNIT_ASSIGNED_CONTEXT((#10628,#10630,#10631))
REPRESENTATION_CONTEXT('','3D')
);
#10604=(
GEOMETRIC_REPRESENTATION_CONTEXT(3)
GLOBAL_UNCERTAINTY_ASSIGNED_CONTEXT((#10572))
GLOBAL_UNIT_ASSIGNED_CONTEXT((#10628,#10630,#10631))
REPRESENTATION_CONTEXT('','3D')
);
#10605=(
GEOMETRIC_REPRESENTATION_CONTEXT(3)
GLOBAL_UNCERTAINTY_ASSIGNED_CONTEXT((#10573))
GLOBAL_UNIT_ASSIGNED_CONTEXT((#10628,#10630,#10631))
REPRESENTATION_CONTEXT('','3D')
);
#10606=(
GEOMETRIC_REPRESENTATION_CONTEXT(3)
GLOBAL_UNCERTAINTY_ASSIGNED_CONTEXT((#10574))
GLOBAL_UNIT_ASSIGNED_CONTEXT((#10628,#10630,#10631))
REPRESENTATION_CONTEXT('','3D')
);
#10607=(
GEOMETRIC_REPRESENTATION_CONTEXT(3)
GLOBAL_UNCERTAINTY_ASSIGNED_CONTEXT((#10575))
GLOBAL_UNIT_ASSIGNED_CONTEXT((#10628,#10630,#10631))
REPRESENTATION_CONTEXT('','3D')
);
#10608=(
GEOMETRIC_REPRESENTATION_CONTEXT(3)
GLOBAL_UNCERTAINTY_ASSIGNED_CONTEXT((#10576))
GLOBAL_UNIT_ASSIGNED_CONTEXT((#10628,#10630,#10631))
REPRESENTATION_CONTEXT('','3D')
);
#10609=(
GEOMETRIC_REPRESENTATION_CONTEXT(3)
GLOBAL_UNCERTAINTY_ASSIGNED_CONTEXT((#10577))
GLOBAL_UNIT_ASSIGNED_CONTEXT((#10628,#10630,#10631))
REPRESENTATION_CONTEXT('','3D')
);
#10610=(
GEOMETRIC_REPRESENTATION_CONTEXT(3)
GLOBAL_UNCERTAINTY_ASSIGNED_CONTEXT((#10578))
GLOBAL_UNIT_ASSIGNED_CONTEXT((#10628,#10630,#10631))
REPRESENTATION_CONTEXT('','3D')
);
#10611=(
GEOMETRIC_REPRESENTATION_CONTEXT(3)
GLOBAL_UNCERTAINTY_ASSIGNED_CONTEXT((#10579))
GLOBAL_UNIT_ASSIGNED_CONTEXT((#10628,#10630,#10631))
REPRESENTATION_CONTEXT('','3D')
);
#10612=(
GEOMETRIC_REPRESENTATION_CONTEXT(3)
GLOBAL_UNCERTAINTY_ASSIGNED_CONTEXT((#10580))
GLOBAL_UNIT_ASSIGNED_CONTEXT((#10628,#10630,#10631))
REPRESENTATION_CONTEXT('','3D')
);
#10613=(
GEOMETRIC_REPRESENTATION_CONTEXT(3)
GLOBAL_UNCERTAINTY_ASSIGNED_CONTEXT((#10581))
GLOBAL_UNIT_ASSIGNED_CONTEXT((#10628,#10630,#10631))
REPRESENTATION_CONTEXT('','3D')
);
#10614=(
GEOMETRIC_REPRESENTATION_CONTEXT(3)
GLOBAL_UNCERTAINTY_ASSIGNED_CONTEXT((#10582))
GLOBAL_UNIT_ASSIGNED_CONTEXT((#10628,#10630,#10631))
REPRESENTATION_CONTEXT('','3D')
);
#10615=(
GEOMETRIC_REPRESENTATION_CONTEXT(3)
GLOBAL_UNCERTAINTY_ASSIGNED_CONTEXT((#10583))
GLOBAL_UNIT_ASSIGNED_CONTEXT((#10628,#10630,#10631))
REPRESENTATION_CONTEXT('','3D')
);
#10616=(
GEOMETRIC_REPRESENTATION_CONTEXT(3)
GLOBAL_UNCERTAINTY_ASSIGNED_CONTEXT((#10584))
GLOBAL_UNIT_ASSIGNED_CONTEXT((#10628,#10630,#10631))
REPRESENTATION_CONTEXT('','3D')
);
#10617=(
GEOMETRIC_REPRESENTATION_CONTEXT(3)
GLOBAL_UNCERTAINTY_ASSIGNED_CONTEXT((#10585))
GLOBAL_UNIT_ASSIGNED_CONTEXT((#10628,#10630,#10631))
REPRESENTATION_CONTEXT('','3D')
);
#10618=(
GEOMETRIC_REPRESENTATION_CONTEXT(3)
GLOBAL_UNCERTAINTY_ASSIGNED_CONTEXT((#10586))
GLOBAL_UNIT_ASSIGNED_CONTEXT((#10628,#10630,#10631))
REPRESENTATION_CONTEXT('','3D')
);
#10619=(
GEOMETRIC_REPRESENTATION_CONTEXT(3)
GLOBAL_UNCERTAINTY_ASSIGNED_CONTEXT((#10587))
GLOBAL_UNIT_ASSIGNED_CONTEXT((#10628,#10630,#10631))
REPRESENTATION_CONTEXT('','3D')
);
#10620=(
GEOMETRIC_REPRESENTATION_CONTEXT(3)
GLOBAL_UNCERTAINTY_ASSIGNED_CONTEXT((#10588))
GLOBAL_UNIT_ASSIGNED_CONTEXT((#10628,#10630,#10631))
REPRESENTATION_CONTEXT('','3D')
);
#10621=(
GEOMETRIC_REPRESENTATION_CONTEXT(3)
GLOBAL_UNCERTAINTY_ASSIGNED_CONTEXT((#10589))
GLOBAL_UNIT_ASSIGNED_CONTEXT((#10628,#10630,#10631))
REPRESENTATION_CONTEXT('','3D')
);
#10622=(
GEOMETRIC_REPRESENTATION_CONTEXT(3)
GLOBAL_UNCERTAINTY_ASSIGNED_CONTEXT((#10590))
GLOBAL_UNIT_ASSIGNED_CONTEXT((#10628,#10630,#10631))
REPRESENTATION_CONTEXT('','3D')
);
#10623=(
GEOMETRIC_REPRESENTATION_CONTEXT(3)
GLOBAL_UNCERTAINTY_ASSIGNED_CONTEXT((#10591))
GLOBAL_UNIT_ASSIGNED_CONTEXT((#10628,#10630,#10631))
REPRESENTATION_CONTEXT('','3D')
);
#10624=(
GEOMETRIC_REPRESENTATION_CONTEXT(3)
GLOBAL_UNCERTAINTY_ASSIGNED_CONTEXT((#10592))
GLOBAL_UNIT_ASSIGNED_CONTEXT((#10628,#10630,#10631))
REPRESENTATION_CONTEXT('','3D')
);
#10625=(
GEOMETRIC_REPRESENTATION_CONTEXT(3)
GLOBAL_UNCERTAINTY_ASSIGNED_CONTEXT((#10593))
GLOBAL_UNIT_ASSIGNED_CONTEXT((#10628,#10630,#10631))
REPRESENTATION_CONTEXT('','3D')
);
#10626=(
GEOMETRIC_REPRESENTATION_CONTEXT(3)
GLOBAL_UNCERTAINTY_ASSIGNED_CONTEXT((#10594))
GLOBAL_UNIT_ASSIGNED_CONTEXT((#10628,#10630,#10631))
REPRESENTATION_CONTEXT('','3D')
);
#10627=(
GEOMETRIC_REPRESENTATION_CONTEXT(3)
GLOBAL_UNCERTAINTY_ASSIGNED_CONTEXT((#10595))
GLOBAL_UNIT_ASSIGNED_CONTEXT((#10628,#10630,#10631))
REPRESENTATION_CONTEXT('','3D')
);
#10628=(
LENGTH_UNIT()
NAMED_UNIT(*)
SI_UNIT(.CENTI.,.METRE.)
);
#10629=(
LENGTH_UNIT()
NAMED_UNIT(*)
SI_UNIT($,.METRE.)
);
#10630=(
NAMED_UNIT(*)
PLANE_ANGLE_UNIT()
SI_UNIT($,.RADIAN.)
);
#10631=(
NAMED_UNIT(*)
SI_UNIT($,.STERADIAN.)
SOLID_ANGLE_UNIT()
);
#10632=SHAPE_DEFINITION_REPRESENTATION(#10663,#10737);
#10633=SHAPE_DEFINITION_REPRESENTATION(#10664,#10738);
#10634=SHAPE_DEFINITION_REPRESENTATION(#10665,#10739);
#10635=SHAPE_DEFINITION_REPRESENTATION(#10666,#10740);
#10636=SHAPE_DEFINITION_REPRESENTATION(#10667,#10741);
#10637=SHAPE_DEFINITION_REPRESENTATION(#10668,#10742);
#10638=SHAPE_DEFINITION_REPRESENTATION(#10669,#10743);
#10639=SHAPE_DEFINITION_REPRESENTATION(#10670,#10744);
#10640=SHAPE_DEFINITION_REPRESENTATION(#10671,#10745);
#10641=SHAPE_DEFINITION_REPRESENTATION(#10682,#10746);
#10642=SHAPE_DEFINITION_REPRESENTATION(#10683,#10747);
#10643=SHAPE_DEFINITION_REPRESENTATION(#10684,#10748);
#10644=SHAPE_DEFINITION_REPRESENTATION(#10685,#10749);
#10645=SHAPE_DEFINITION_REPRESENTATION(#10686,#10750);
#10646=SHAPE_DEFINITION_REPRESENTATION(#10687,#10751);
#10647=SHAPE_DEFINITION_REPRESENTATION(#10688,#10752);
#10648=SHAPE_DEFINITION_REPRESENTATION(#10689,#10753);
#10649=SHAPE_DEFINITION_REPRESENTATION(#10690,#10754);
#10650=SHAPE_DEFINITION_REPRESENTATION(#10691,#10755);
#10651=SHAPE_DEFINITION_REPRESENTATION(#10692,#10756);
#10652=SHAPE_DEFINITION_REPRESENTATION(#10693,#10757);
#10653=SHAPE_DEFINITION_REPRESENTATION(#10694,#10758);
#10654=SHAPE_DEFINITION_REPRESENTATION(#10695,#10759);
#10655=SHAPE_DEFINITION_REPRESENTATION(#10701,#10760);
#10656=SHAPE_DEFINITION_REPRESENTATION(#10702,#10761);
#10657=SHAPE_DEFINITION_REPRESENTATION(#10703,#10762);
#10658=SHAPE_DEFINITION_REPRESENTATION(#10704,#10763);
#10659=SHAPE_DEFINITION_REPRESENTATION(#10705,#10764);
#10660=SHAPE_DEFINITION_REPRESENTATION(#10706,#10765);
#10661=SHAPE_DEFINITION_REPRESENTATION(#10707,#10766);
#10662=SHAPE_DEFINITION_REPRESENTATION(#10708,#10767);
#10663=PRODUCT_DEFINITION_SHAPE('',$,#10769);
#10664=PRODUCT_DEFINITION_SHAPE('',$,#10770);
#10665=PRODUCT_DEFINITION_SHAPE('',$,#10771);
#10666=PRODUCT_DEFINITION_SHAPE('',$,#10772);
#10667=PRODUCT_DEFINITION_SHAPE('',$,#10773);
#10668=PRODUCT_DEFINITION_SHAPE('',$,#10774);
#10669=PRODUCT_DEFINITION_SHAPE('',$,#10775);
#10670=PRODUCT_DEFINITION_SHAPE('',$,#10776);
#10671=PRODUCT_DEFINITION_SHAPE('',$,#10777);
#10672=PRODUCT_DEFINITION_SHAPE($,$,#158);
#10673=PRODUCT_DEFINITION_SHAPE($,$,#159);
#10674=PRODUCT_DEFINITION_SHAPE($,$,#160);
#10675=PRODUCT_DEFINITION_SHAPE($,$,#161);
#10676=PRODUCT_DEFINITION_SHAPE($,$,#162);
#10677=PRODUCT_DEFINITION_SHAPE($,$,#163);
#10678=PRODUCT_DEFINITION_SHAPE($,$,#164);
#10679=PRODUCT_DEFINITION_SHAPE($,$,#165);
#10680=PRODUCT_DEFINITION_SHAPE($,$,#166);
#10681=PRODUCT_DEFINITION_SHAPE($,$,#167);
#10682=PRODUCT_DEFINITION_SHAPE('',$,#10778);
#10683=PRODUCT_DEFINITION_SHAPE('',$,#10779);
#10684=PRODUCT_DEFINITION_SHAPE('',$,#10780);
#10685=PRODUCT_DEFINITION_SHAPE('',$,#10781);
#10686=PRODUCT_DEFINITION_SHAPE('',$,#10782);
#10687=PRODUCT_DEFINITION_SHAPE('',$,#10783);
#10688=PRODUCT_DEFINITION_SHAPE('',$,#10784);
#10689=PRODUCT_DEFINITION_SHAPE('',$,#10785);
#10690=PRODUCT_DEFINITION_SHAPE('',$,#10786);
#10691=PRODUCT_DEFINITION_SHAPE('',$,#10787);
#10692=PRODUCT_DEFINITION_SHAPE('',$,#10788);
#10693=PRODUCT_DEFINITION_SHAPE('',$,#10789);
#10694=PRODUCT_DEFINITION_SHAPE('',$,#10790);
#10695=PRODUCT_DEFINITION_SHAPE('',$,#10791);
#10696=PRODUCT_DEFINITION_SHAPE($,$,#168);
#10697=PRODUCT_DEFINITION_SHAPE($,$,#169);
#10698=PRODUCT_DEFINITION_SHAPE($,$,#170);
#10699=PRODUCT_DEFINITION_SHAPE($,$,#171);
#10700=PRODUCT_DEFINITION_SHAPE($,$,#172);
#10701=PRODUCT_DEFINITION_SHAPE('',$,#10792);
#10702=PRODUCT_DEFINITION_SHAPE('',$,#10793);
#10703=PRODUCT_DEFINITION_SHAPE('',$,#10794);
#10704=PRODUCT_DEFINITION_SHAPE('',$,#10795);
#10705=PRODUCT_DEFINITION_SHAPE('',$,#10796);
#10706=PRODUCT_DEFINITION_SHAPE('',$,#10797);
#10707=PRODUCT_DEFINITION_SHAPE('',$,#10798);
#10708=PRODUCT_DEFINITION_SHAPE('',$,#10799);
#10709=PRODUCT_DEFINITION_SHAPE($,$,#173);
#10710=PRODUCT_DEFINITION_SHAPE($,$,#174);
#10711=PRODUCT_DEFINITION_SHAPE($,$,#175);
#10712=PRODUCT_DEFINITION_SHAPE($,$,#176);
#10713=PRODUCT_DEFINITION_SHAPE($,$,#177);
#10714=PRODUCT_DEFINITION_SHAPE($,$,#178);
#10715=PRODUCT_DEFINITION_SHAPE($,$,#179);
#10716=PRODUCT_DEFINITION_SHAPE($,$,#180);
#10717=PRODUCT_DEFINITION_SHAPE($,$,#181);
#10718=PRODUCT_DEFINITION_SHAPE($,$,#182);
#10719=PRODUCT_DEFINITION_SHAPE($,$,#183);
#10720=PRODUCT_DEFINITION_SHAPE($,$,#184);
#10721=PRODUCT_DEFINITION_SHAPE($,$,#185);
#10722=PRODUCT_DEFINITION_SHAPE($,$,#186);
#10723=PRODUCT_DEFINITION_SHAPE($,$,#187);
#10724=PRODUCT_DEFINITION_SHAPE($,$,#188);
#10725=PRODUCT_DEFINITION_SHAPE($,$,#189);
#10726=PRODUCT_DEFINITION_SHAPE($,$,#190);
#10727=PRODUCT_DEFINITION_SHAPE($,$,#191);
#10728=PRODUCT_DEFINITION_SHAPE($,$,#192);
#10729=PRODUCT_DEFINITION_SHAPE($,$,#193);
#10730=PRODUCT_DEFINITION_SHAPE($,$,#194);
#10731=PRODUCT_DEFINITION_SHAPE($,$,#195);
#10732=PRODUCT_DEFINITION_SHAPE($,$,#196);
#10733=PRODUCT_DEFINITION_SHAPE($,$,#197);
#10734=PRODUCT_DEFINITION_SHAPE($,$,#198);
#10735=PRODUCT_DEFINITION_SHAPE($,$,#199);
#10736=PRODUCT_DEFINITION_SHAPE($,$,#200);
#10737=SHAPE_REPRESENTATION('',(#5223,#5867,#5868,#5869),#10596);
#10738=SHAPE_REPRESENTATION('',(#5224,#5395,#5396,#5397,#5398,#5399,#5400,
#5401,#5402,#5403,#5404),#10597);
#10739=SHAPE_REPRESENTATION('',(#5225),#10598);
#10740=SHAPE_REPRESENTATION('',(#5244),#10599);
#10741=SHAPE_REPRESENTATION('',(#5251),#10600);
#10742=SHAPE_REPRESENTATION('',(#5258),#10601);
#10743=SHAPE_REPRESENTATION('',(#5359),#10602);
#10744=SHAPE_REPRESENTATION('',(#5366),#10603);
#10745=SHAPE_REPRESENTATION('',(#5371),#10604);
#10746=SHAPE_REPRESENTATION('',(#5405,#5842,#5843,#5844,#5845,#5846,#5847,
#5848,#5849,#5850,#5851,#5852,#5853,#5854,#5855,#5856,#5857,#5858),#10605);
#10747=SHAPE_REPRESENTATION('',(#5406),#10606);
#10748=SHAPE_REPRESENTATION('',(#5460),#10607);
#10749=SHAPE_REPRESENTATION('',(#5469),#10608);
#10750=SHAPE_REPRESENTATION('',(#5478),#10609);
#10751=SHAPE_REPRESENTATION('',(#5519),#10610);
#10752=SHAPE_REPRESENTATION('',(#5563),#10611);
#10753=SHAPE_REPRESENTATION('',(#5573),#10612);
#10754=SHAPE_REPRESENTATION('',(#5579,#5708,#5709,#5710,#5711,#5712),#10613);
#10755=SHAPE_REPRESENTATION('',(#5580),#10614);
#10756=SHAPE_REPRESENTATION('',(#5600),#10615);
#10757=SHAPE_REPRESENTATION('',(#5620),#10616);
#10758=SHAPE_REPRESENTATION('',(#5637),#10617);
#10759=SHAPE_REPRESENTATION('',(#5691),#10618);
#10760=SHAPE_REPRESENTATION('',(#5713,#5859,#5860,#5861,#5862,#5863,#5864,
#5865,#5866),#10619);
#10761=SHAPE_REPRESENTATION('',(#5714),#10620);
#10762=SHAPE_REPRESENTATION('',(#5744),#10621);
#10763=SHAPE_REPRESENTATION('',(#5764),#10622);
#10764=SHAPE_REPRESENTATION('',(#5774),#10623);
#10765=SHAPE_REPRESENTATION('',(#5783),#10624);
#10766=SHAPE_REPRESENTATION('',(#5792),#10625);
#10767=SHAPE_REPRESENTATION('',(#5818),#10626);
#10768=PRODUCT_DEFINITION_CONTEXT('part definition',#10863,'design');
#10769=PRODUCT_DEFINITION('PAT-102','PAT-102',#10800,#10768);
#10770=PRODUCT_DEFINITION('Base, post and cam fork',
'Base, post and cam fork',#10801,#10768);
#10771=PRODUCT_DEFINITION('Base','Base',#10802,#10768);
#10772=PRODUCT_DEFINITION('Foot strip','Foot strip',#10803,#10768);
#10773=PRODUCT_DEFINITION('Foot strip (1)','Foot strip (1)',#10804,#10768);
#10774=PRODUCT_DEFINITION('Post and cam fork','Post and cam fork',#10805,
#10768);
#10775=PRODUCT_DEFINITION('Workpiece envelope','Workpiece envelope',#10806,
#10768);
#10776=PRODUCT_DEFINITION('Installed lift spring',
'Installed lift spring',#10807,#10768);
#10777=PRODUCT_DEFINITION('M5x14 Cap Screw','M5x14 Cap Screw',#10808,#10768);
#10778=PRODUCT_DEFINITION('Swinging clamp arm','Swinging clamp arm',#10809,
#10768);
#10779=PRODUCT_DEFINITION('Arm and bearing sleeve',
'Arm and bearing sleeve',#10810,#10768);
#10780=PRODUCT_DEFINITION('Outer race separator','Outer race separator',
#10811,#10768);
#10781=PRODUCT_DEFINITION('Inner race separator','Inner race separator',
#10812,#10768);
#10782=PRODUCT_DEFINITION('Lower bearing cap','Lower bearing cap',#10813,
#10768);
#10783=PRODUCT_DEFINITION('Cam contact cap','Cam contact cap',#10814,#10768);
#10784=PRODUCT_DEFINITION('Pressure shoe','Pressure shoe',#10815,#10768);
#10785=PRODUCT_DEFINITION('Compliant pressure pad',
'Compliant pressure pad',#10816,#10768);
#10786=PRODUCT_DEFINITION('Sealed Ball Bearing - 10 x 30 x 9 mm',
'Sealed Ball Bearing - 10 x 30 x 9 mm',#10817,#10768);
#10787=PRODUCT_DEFINITION('Inner ring','Inner ring',#10818,#10768);
#10788=PRODUCT_DEFINITION('Outer ring','Outer ring',#10819,#10768);
#10789=PRODUCT_DEFINITION('Balls','Balls',#10820,#10768);
#10790=PRODUCT_DEFINITION('Cage','Cage',#10821,#10768);
#10791=PRODUCT_DEFINITION('Seals 2RS','Seals 2RS',#10822,#10768);
#10792=PRODUCT_DEFINITION('Eccentric cam and lever',
'Eccentric cam and lever',#10823,#10768);
#10793=PRODUCT_DEFINITION('Eccentric cam and axle',
'Eccentric cam and axle',#10824,#10768);
#10794=PRODUCT_DEFINITION('Cam lever','Cam lever',#10825,#10768);
#10795=PRODUCT_DEFINITION('Lever grip','Lever grip',#10826,#10768);
#10796=PRODUCT_DEFINITION('Cam axle keeper','Cam axle keeper',#10827,#10768);
#10797=PRODUCT_DEFINITION('Cam axle keeper (1)','Cam axle keeper (1)',#10828,
#10768);
#10798=PRODUCT_DEFINITION('Cap Screw - M4x16','Cap Screw - M4x16',#10829,
#10768);
#10799=PRODUCT_DEFINITION('M4x10 Cap Screw','M4x10 Cap Screw',#10830,#10768);
#10800=PRODUCT_DEFINITION_FORMATION('',$,#10865);
#10801=PRODUCT_DEFINITION_FORMATION('',$,#10866);
#10802=PRODUCT_DEFINITION_FORMATION('',$,#10867);
#10803=PRODUCT_DEFINITION_FORMATION('',$,#10868);
#10804=PRODUCT_DEFINITION_FORMATION('',$,#10869);
#10805=PRODUCT_DEFINITION_FORMATION('',$,#10870);
#10806=PRODUCT_DEFINITION_FORMATION('',$,#10871);
#10807=PRODUCT_DEFINITION_FORMATION('',$,#10872);
#10808=PRODUCT_DEFINITION_FORMATION('',$,#10873);
#10809=PRODUCT_DEFINITION_FORMATION('',$,#10874);
#10810=PRODUCT_DEFINITION_FORMATION('',$,#10875);
#10811=PRODUCT_DEFINITION_FORMATION('',$,#10876);
#10812=PRODUCT_DEFINITION_FORMATION('',$,#10877);
#10813=PRODUCT_DEFINITION_FORMATION('',$,#10878);
#10814=PRODUCT_DEFINITION_FORMATION('',$,#10879);
#10815=PRODUCT_DEFINITION_FORMATION('',$,#10880);
#10816=PRODUCT_DEFINITION_FORMATION('',$,#10881);
#10817=PRODUCT_DEFINITION_FORMATION('',$,#10882);
#10818=PRODUCT_DEFINITION_FORMATION('',$,#10883);
#10819=PRODUCT_DEFINITION_FORMATION('',$,#10884);
#10820=PRODUCT_DEFINITION_FORMATION('',$,#10885);
#10821=PRODUCT_DEFINITION_FORMATION('',$,#10886);
#10822=PRODUCT_DEFINITION_FORMATION('',$,#10887);
#10823=PRODUCT_DEFINITION_FORMATION('',$,#10888);
#10824=PRODUCT_DEFINITION_FORMATION('',$,#10889);
#10825=PRODUCT_DEFINITION_FORMATION('',$,#10890);
#10826=PRODUCT_DEFINITION_FORMATION('',$,#10891);
#10827=PRODUCT_DEFINITION_FORMATION('',$,#10892);
#10828=PRODUCT_DEFINITION_FORMATION('',$,#10893);
#10829=PRODUCT_DEFINITION_FORMATION('',$,#10894);
#10830=PRODUCT_DEFINITION_FORMATION('',$,#10895);
#10831=PRODUCT_RELATED_PRODUCT_CATEGORY('PAT-102','PAT-102',(#10865));
#10832=PRODUCT_RELATED_PRODUCT_CATEGORY('Base, post and cam fork',
'Base, post and cam fork',(#10866));
#10833=PRODUCT_RELATED_PRODUCT_CATEGORY('Base','Base',(#10867));
#10834=PRODUCT_RELATED_PRODUCT_CATEGORY('Foot strip','Foot strip',(#10868));
#10835=PRODUCT_RELATED_PRODUCT_CATEGORY('Foot strip (1)',
'Foot strip (1)',(#10869));
#10836=PRODUCT_RELATED_PRODUCT_CATEGORY('Post and cam fork',
'Post and cam fork',(#10870));
#10837=PRODUCT_RELATED_PRODUCT_CATEGORY('Workpiece envelope',
'Workpiece envelope',(#10871));
#10838=PRODUCT_RELATED_PRODUCT_CATEGORY('Installed lift spring',
'Installed lift spring',(#10872));
#10839=PRODUCT_RELATED_PRODUCT_CATEGORY('M5x14 Cap Screw',
'M5x14 Cap Screw',(#10873));
#10840=PRODUCT_RELATED_PRODUCT_CATEGORY('Swinging clamp arm',
'Swinging clamp arm',(#10874));
#10841=PRODUCT_RELATED_PRODUCT_CATEGORY('Arm and bearing sleeve',
'Arm and bearing sleeve',(#10875));
#10842=PRODUCT_RELATED_PRODUCT_CATEGORY('Outer race separator',
'Outer race separator',(#10876));
#10843=PRODUCT_RELATED_PRODUCT_CATEGORY('Inner race separator',
'Inner race separator',(#10877));
#10844=PRODUCT_RELATED_PRODUCT_CATEGORY('Lower bearing cap',
'Lower bearing cap',(#10878));
#10845=PRODUCT_RELATED_PRODUCT_CATEGORY('Cam contact cap',
'Cam contact cap',(#10879));
#10846=PRODUCT_RELATED_PRODUCT_CATEGORY('Pressure shoe','Pressure shoe',
(#10880));
#10847=PRODUCT_RELATED_PRODUCT_CATEGORY('Compliant pressure pad',
'Compliant pressure pad',(#10881));
#10848=PRODUCT_RELATED_PRODUCT_CATEGORY(
'Sealed Ball Bearing - 10 x 30 x 9 mm',
'Sealed Ball Bearing - 10 x 30 x 9 mm',(#10882));
#10849=PRODUCT_RELATED_PRODUCT_CATEGORY('Inner ring','Inner ring',(#10883));
#10850=PRODUCT_RELATED_PRODUCT_CATEGORY('Outer ring','Outer ring',(#10884));
#10851=PRODUCT_RELATED_PRODUCT_CATEGORY('Balls','Balls',(#10885));
#10852=PRODUCT_RELATED_PRODUCT_CATEGORY('Cage','Cage',(#10886));
#10853=PRODUCT_RELATED_PRODUCT_CATEGORY('Seals 2RS','Seals 2RS',(#10887));
#10854=PRODUCT_RELATED_PRODUCT_CATEGORY('Eccentric cam and lever',
'Eccentric cam and lever',(#10888));
#10855=PRODUCT_RELATED_PRODUCT_CATEGORY('Eccentric cam and axle',
'Eccentric cam and axle',(#10889));
#10856=PRODUCT_RELATED_PRODUCT_CATEGORY('Cam lever','Cam lever',(#10890));
#10857=PRODUCT_RELATED_PRODUCT_CATEGORY('Lever grip','Lever grip',(#10891));
#10858=PRODUCT_RELATED_PRODUCT_CATEGORY('Cam axle keeper',
'Cam axle keeper',(#10892));
#10859=PRODUCT_RELATED_PRODUCT_CATEGORY('Cam axle keeper (1)',
'Cam axle keeper (1)',(#10893));
#10860=PRODUCT_RELATED_PRODUCT_CATEGORY('Cap Screw - M4x16',
'Cap Screw - M4x16',(#10894));
#10861=PRODUCT_RELATED_PRODUCT_CATEGORY('M4x10 Cap Screw',
'M4x10 Cap Screw',(#10895));
#10862=APPLICATION_PROTOCOL_DEFINITION('international standard',
'automotive_design',2009,#10863);
#10863=APPLICATION_CONTEXT(
'Core Data for Automotive Mechanical Design Process');
#10864=PRODUCT_CONTEXT('part definition',#10863,'mechanical');
#10865=PRODUCT('PAT-102','PAT-102','PAT-102',
(#10864));
#10866=PRODUCT('Base, post and cam fork','Base, post and cam fork',
'Base, post and cam fork',(#10864));
#10867=PRODUCT('Base','Base','Base',(#10864));
#10868=PRODUCT('Foot strip','Foot strip','Foot strip',(#10864));
#10869=PRODUCT('Foot strip (1)','Foot strip (1)','Foot strip (1)',(#10864));
#10870=PRODUCT('Post and cam fork','Post and cam fork',
'Post and cam fork',(#10864));
#10871=PRODUCT('Workpiece envelope','Workpiece envelope',
'Workpiece envelope',(#10864));
#10872=PRODUCT('Installed lift spring','Installed lift spring',
'Installed lift spring',(#10864));
#10873=PRODUCT('M5x14 Cap Screw','M5x14 Cap Screw','M5x14 Cap Screw',(#10864));
#10874=PRODUCT('Swinging clamp arm','Swinging clamp arm',
'Swinging clamp arm',(#10864));
#10875=PRODUCT('Arm and bearing sleeve','Arm and bearing sleeve',
'Arm and bearing sleeve',(#10864));
#10876=PRODUCT('Outer race separator','Outer race separator',
'Outer race separator',(#10864));
#10877=PRODUCT('Inner race separator','Inner race separator',
'Inner race separator',(#10864));
#10878=PRODUCT('Lower bearing cap','Lower bearing cap',
'Lower bearing cap',(#10864));
#10879=PRODUCT('Cam contact cap','Cam contact cap','Cam contact cap',(#10864));
#10880=PRODUCT('Pressure shoe','Pressure shoe','Pressure shoe',(#10864));
#10881=PRODUCT('Compliant pressure pad','Compliant pressure pad',
'Compliant pressure pad',(#10864));
#10882=PRODUCT('Sealed Ball Bearing - 10 x 30 x 9 mm',
'Sealed Ball Bearing - 10 x 30 x 9 mm',
'Sealed Ball Bearing - 10 x 30 x 9 mm',(#10864));
#10883=PRODUCT('Inner ring','Inner ring','Inner ring',(#10864));
#10884=PRODUCT('Outer ring','Outer ring','Outer ring',(#10864));
#10885=PRODUCT('Balls','Balls','Balls',(#10864));
#10886=PRODUCT('Cage','Cage','Cage',(#10864));
#10887=PRODUCT('Seals 2RS','Seals 2RS','Seals 2RS',(#10864));
#10888=PRODUCT('Eccentric cam and lever','Eccentric cam and lever',
'Eccentric cam and lever',(#10864));
#10889=PRODUCT('Eccentric cam and axle','Eccentric cam and axle',
'Eccentric cam and axle',(#10864));
#10890=PRODUCT('Cam lever','Cam lever','Cam lever',(#10864));
#10891=PRODUCT('Lever grip','Lever grip','Lever grip',(#10864));
#10892=PRODUCT('Cam axle keeper','Cam axle keeper','Cam axle keeper',(#10864));
#10893=PRODUCT('Cam axle keeper (1)','Cam axle keeper (1)',
'Cam axle keeper (1)',(#10864));
#10894=PRODUCT('Cap Screw - M4x16','Cap Screw - M4x16',
'Cap Screw - M4x16',(#10864));
#10895=PRODUCT('M4x10 Cap Screw','M4x10 Cap Screw','M4x10 Cap Screw',(#10864));
#10896=PRESENTATION_STYLE_ASSIGNMENT((#10902));
#10897=PRESENTATION_STYLE_ASSIGNMENT((#10903));
#10898=PRESENTATION_STYLE_ASSIGNMENT((#10904));
#10899=PRESENTATION_STYLE_ASSIGNMENT((#10905));
#10900=PRESENTATION_STYLE_ASSIGNMENT((#10906));
#10901=PRESENTATION_STYLE_ASSIGNMENT((#10907));
#10902=SURFACE_STYLE_USAGE(.BOTH.,#10908);
#10903=SURFACE_STYLE_USAGE(.BOTH.,#10909);
#10904=SURFACE_STYLE_USAGE(.BOTH.,#10910);
#10905=SURFACE_STYLE_USAGE(.BOTH.,#10911);
#10906=SURFACE_STYLE_USAGE(.BOTH.,#10912);
#10907=SURFACE_STYLE_USAGE(.BOTH.,#10913);
#10908=SURFACE_SIDE_STYLE('',(#10914));
#10909=SURFACE_SIDE_STYLE('',(#10915));
#10910=SURFACE_SIDE_STYLE('',(#10916));
#10911=SURFACE_SIDE_STYLE('',(#10917));
#10912=SURFACE_SIDE_STYLE('',(#10918));
#10913=SURFACE_SIDE_STYLE('',(#10919));
#10914=SURFACE_STYLE_FILL_AREA(#10920);
#10915=SURFACE_STYLE_FILL_AREA(#10921);
#10916=SURFACE_STYLE_FILL_AREA(#10922);
#10917=SURFACE_STYLE_FILL_AREA(#10923);
#10918=SURFACE_STYLE_FILL_AREA(#10924);
#10919=SURFACE_STYLE_FILL_AREA(#10925);
#10920=FILL_AREA_STYLE('Steel - Satin',(#10926));
#10921=FILL_AREA_STYLE('CAD Library Painted - Deep blue',(#10927));
#10922=FILL_AREA_STYLE('CAD Library Painted - Engineering blue',(#10928));
#10923=FILL_AREA_STYLE('CAD Library Painted - Steel gray',(#10929));
#10924=FILL_AREA_STYLE('CAD Library Painted - Graphite',(#10930));
#10925=FILL_AREA_STYLE('CAD Library Painted - Light blue',(#10931));
#10926=FILL_AREA_STYLE_COLOUR('Steel - Satin',#10932);
#10927=FILL_AREA_STYLE_COLOUR('CAD Library Painted - Deep blue',#10933);
#10928=FILL_AREA_STYLE_COLOUR('CAD Library Painted - Engineering blue',
#10934);
#10929=FILL_AREA_STYLE_COLOUR('CAD Library Painted - Steel gray',#10935);
#10930=FILL_AREA_STYLE_COLOUR('CAD Library Painted - Graphite',#10936);
#10931=FILL_AREA_STYLE_COLOUR('CAD Library Painted - Light blue',#10937);
#10932=COLOUR_RGB('Steel - Satin',0.627450980392157,0.627450980392157,0.627450980392157);
#10933=COLOUR_RGB('CAD Library Painted - Deep blue',0.0784313725490196,
0.203921568627451,0.349019607843137);
#10934=COLOUR_RGB('CAD Library Painted - Engineering blue',0.12156862745098,
0.356862745098039,0.6);
#10935=COLOUR_RGB('CAD Library Painted - Steel gray',0.592156862745098,
0.631372549019608,0.67843137254902);
#10936=COLOUR_RGB('CAD Library Painted - Graphite',0.168627450980392,0.192156862745098,
0.231372549019608);
#10937=COLOUR_RGB('CAD Library Painted - Light blue',0.286274509803922,
0.552941176470588,0.780392156862745);
#10938=COLOUR_RGB('Dark Blue',0.08,0.2,0.34);
#10939=FILL_AREA_STYLE_COLOUR('',#10938);
#10940=FILL_AREA_STYLE('',(#10939));
#10941=SURFACE_STYLE_FILL_AREA(#10940);
#10942=SURFACE_SIDE_STYLE('',(#10941));
#10943=SURFACE_STYLE_USAGE(.BOTH.,#10942);
#10944=PRESENTATION_STYLE_ASSIGNMENT((#10943));
#10945=COLOUR_RGB('Light Blue',0.38,0.62,0.78);
#10946=FILL_AREA_STYLE_COLOUR('',#10945);
#10947=FILL_AREA_STYLE('',(#10946));
#10948=SURFACE_STYLE_FILL_AREA(#10947);
#10949=SURFACE_SIDE_STYLE('',(#10948));
#10950=SURFACE_STYLE_USAGE(.BOTH.,#10949);
#10951=PRESENTATION_STYLE_ASSIGNMENT((#10950));
#10952=COLOUR_RGB('Sky Blue',0.24,0.69,0.87);
#10953=FILL_AREA_STYLE_COLOUR('',#10952);
#10954=FILL_AREA_STYLE('',(#10953));
#10955=SURFACE_STYLE_FILL_AREA(#10954);
#10956=SURFACE_SIDE_STYLE('',(#10955));
#10957=SURFACE_STYLE_USAGE(.BOTH.,#10956);
#10958=PRESENTATION_STYLE_ASSIGNMENT((#10957));
#10959=COLOUR_RGB('Grey',0.48,0.52,0.57);
#10960=FILL_AREA_STYLE_COLOUR('',#10959);
#10961=FILL_AREA_STYLE('',(#10960));
#10962=SURFACE_STYLE_FILL_AREA(#10961);
#10963=SURFACE_SIDE_STYLE('',(#10962));
#10964=SURFACE_STYLE_USAGE(.BOTH.,#10963);
#10965=PRESENTATION_STYLE_ASSIGNMENT((#10964));
#10966=COLOUR_RGB('Black',0.12,0.14,0.17);
#10967=FILL_AREA_STYLE_COLOUR('',#10966);
#10968=FILL_AREA_STYLE('',(#10967));
#10969=SURFACE_STYLE_FILL_AREA(#10968);
#10970=SURFACE_SIDE_STYLE('',(#10969));
#10971=SURFACE_STYLE_USAGE(.BOTH.,#10970);
#10972=PRESENTATION_STYLE_ASSIGNMENT((#10971));
#10973=COLOUR_RGB('Off White',0.89,0.88,0.83);
#10974=FILL_AREA_STYLE_COLOUR('',#10973);
#10975=FILL_AREA_STYLE('',(#10974));
#10976=SURFACE_STYLE_FILL_AREA(#10975);
#10977=SURFACE_SIDE_STYLE('',(#10976));
#10978=SURFACE_STYLE_USAGE(.BOTH.,#10977);
#10979=PRESENTATION_STYLE_ASSIGNMENT((#10978));
ENDSEC;
END-ISO-10303-21;
